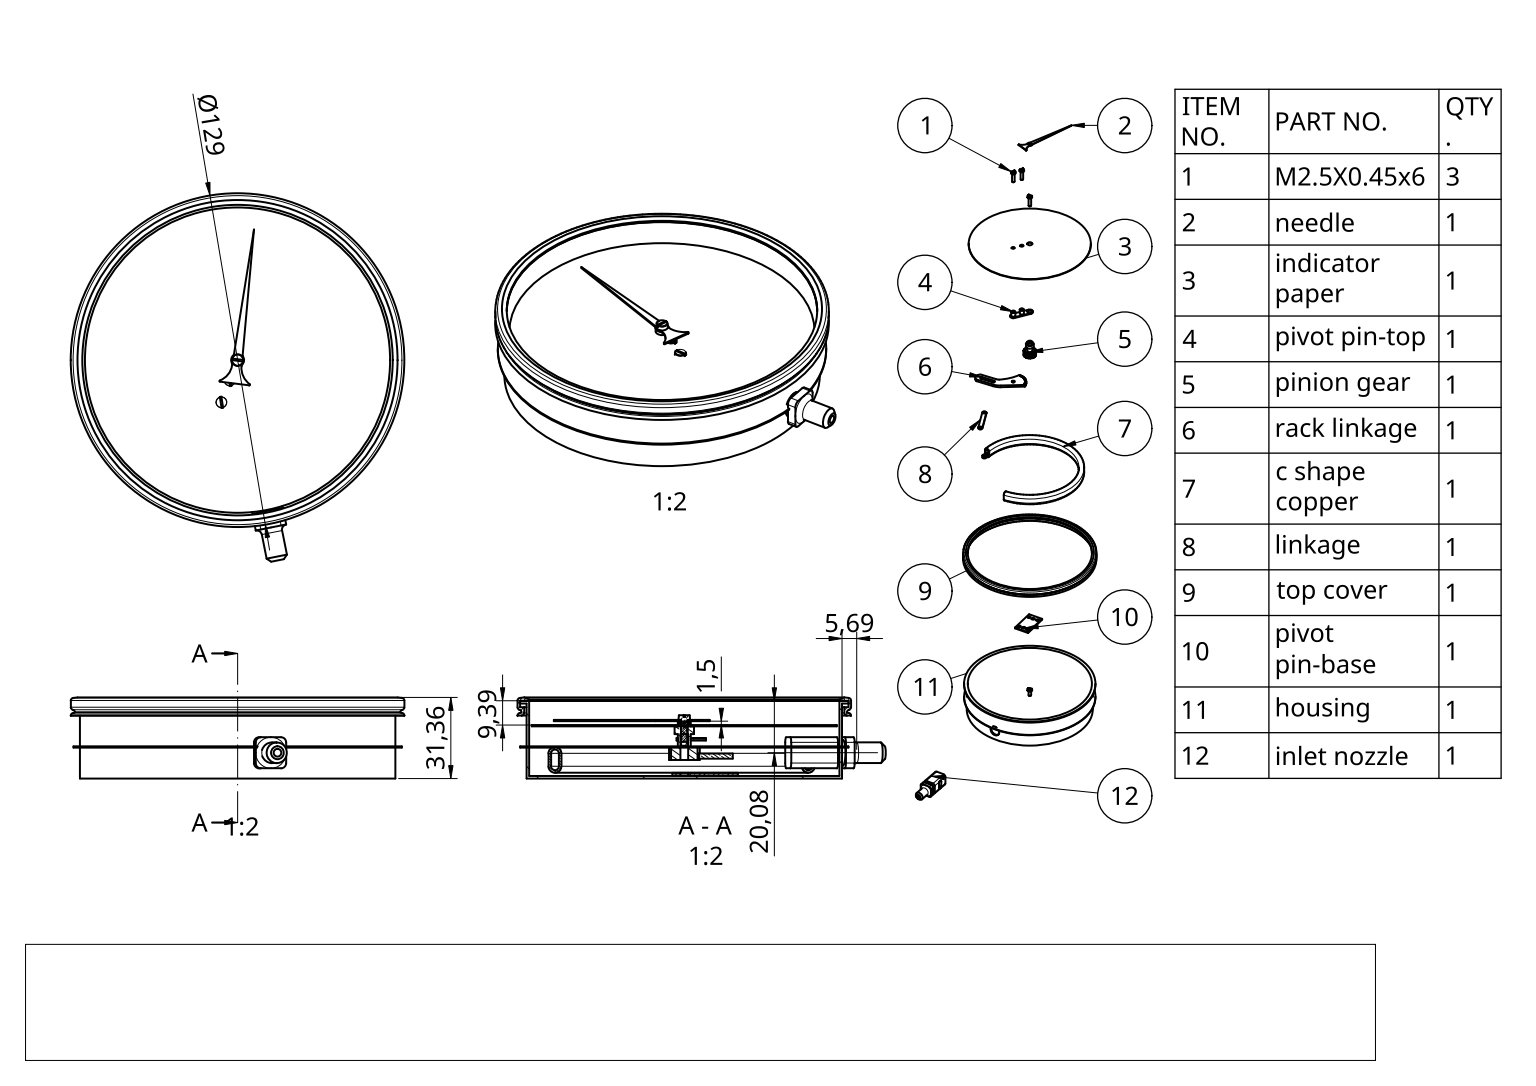
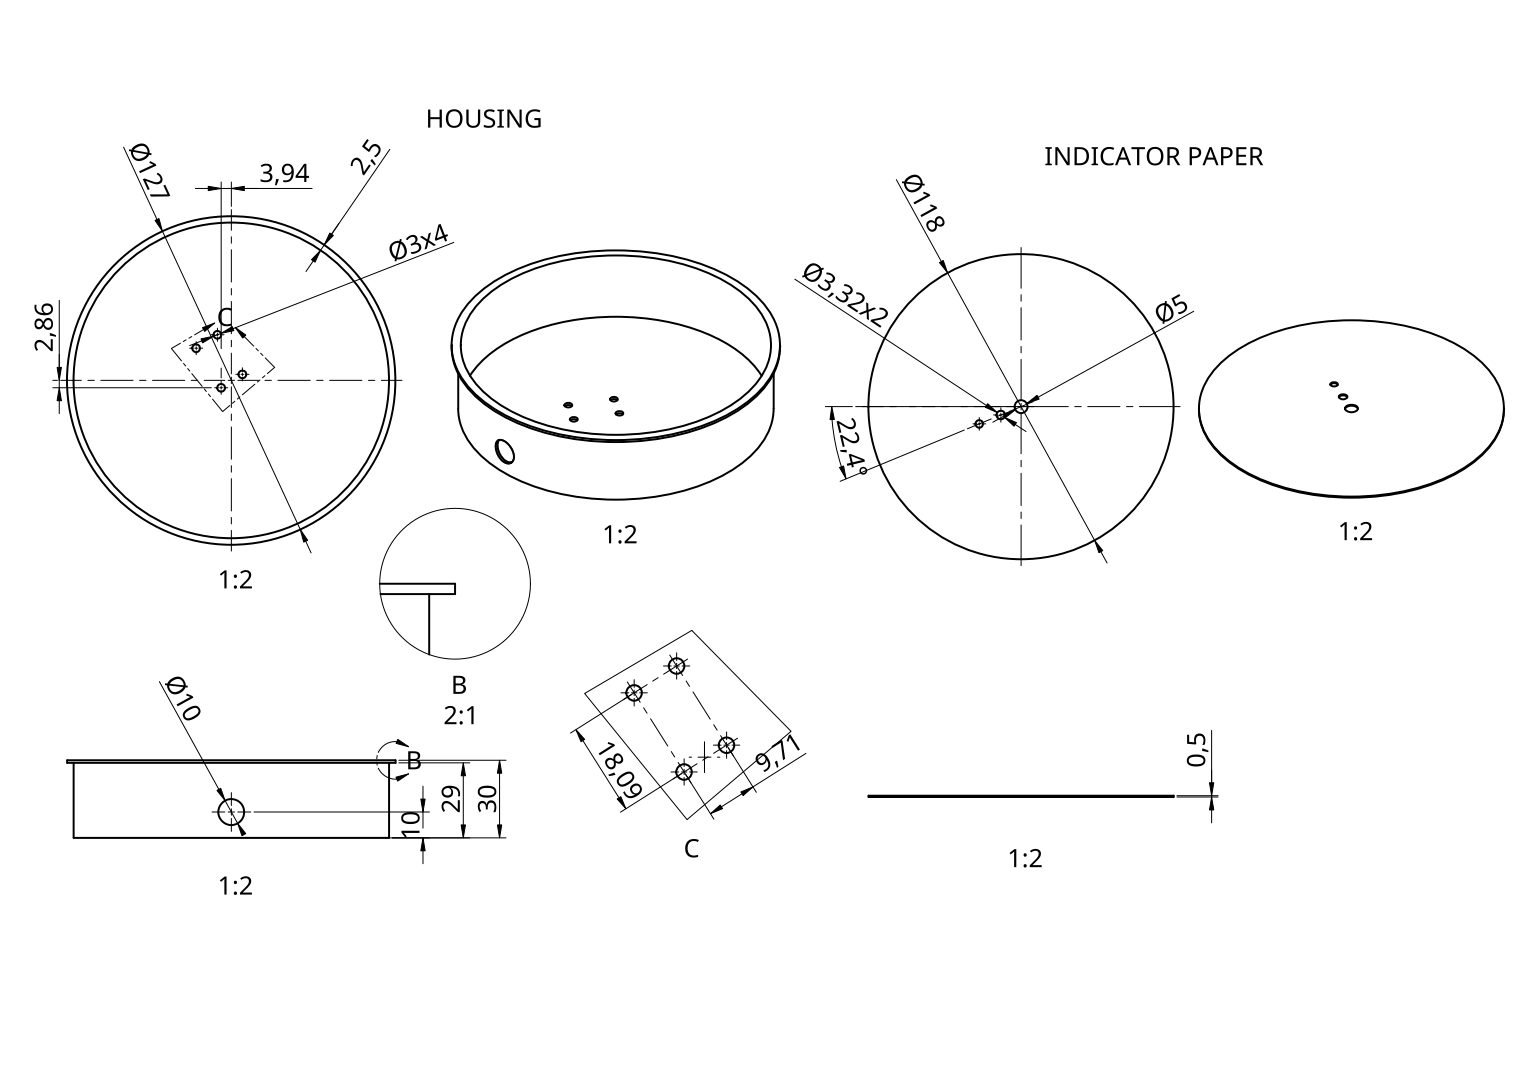
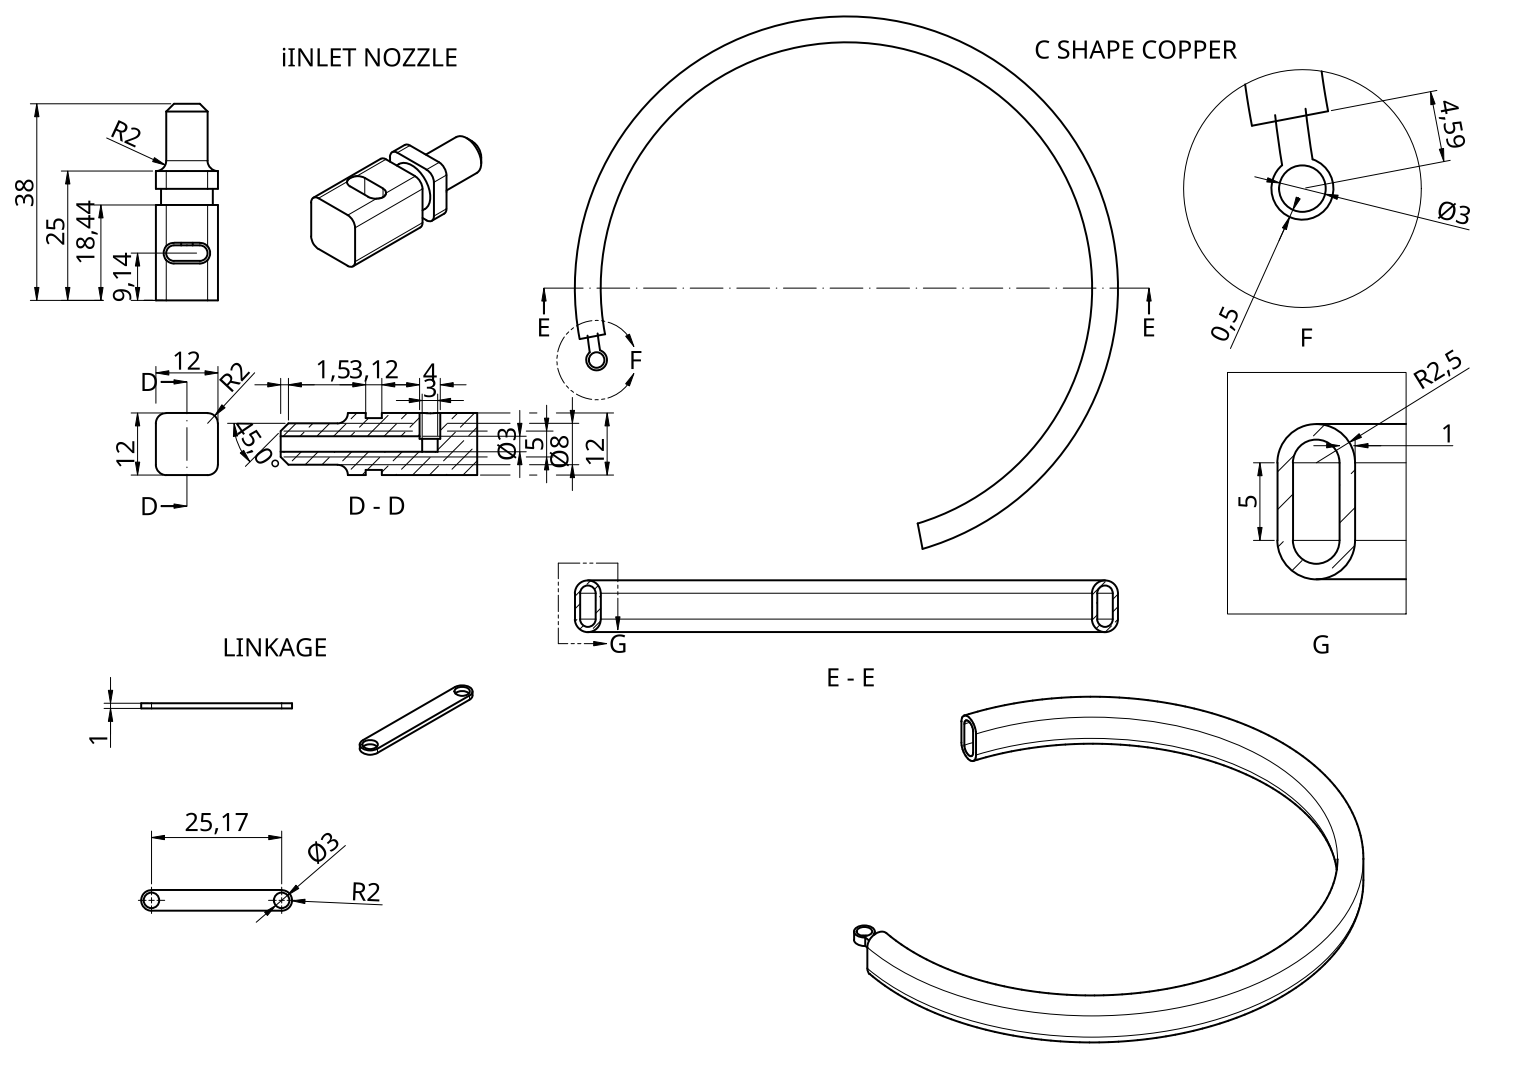
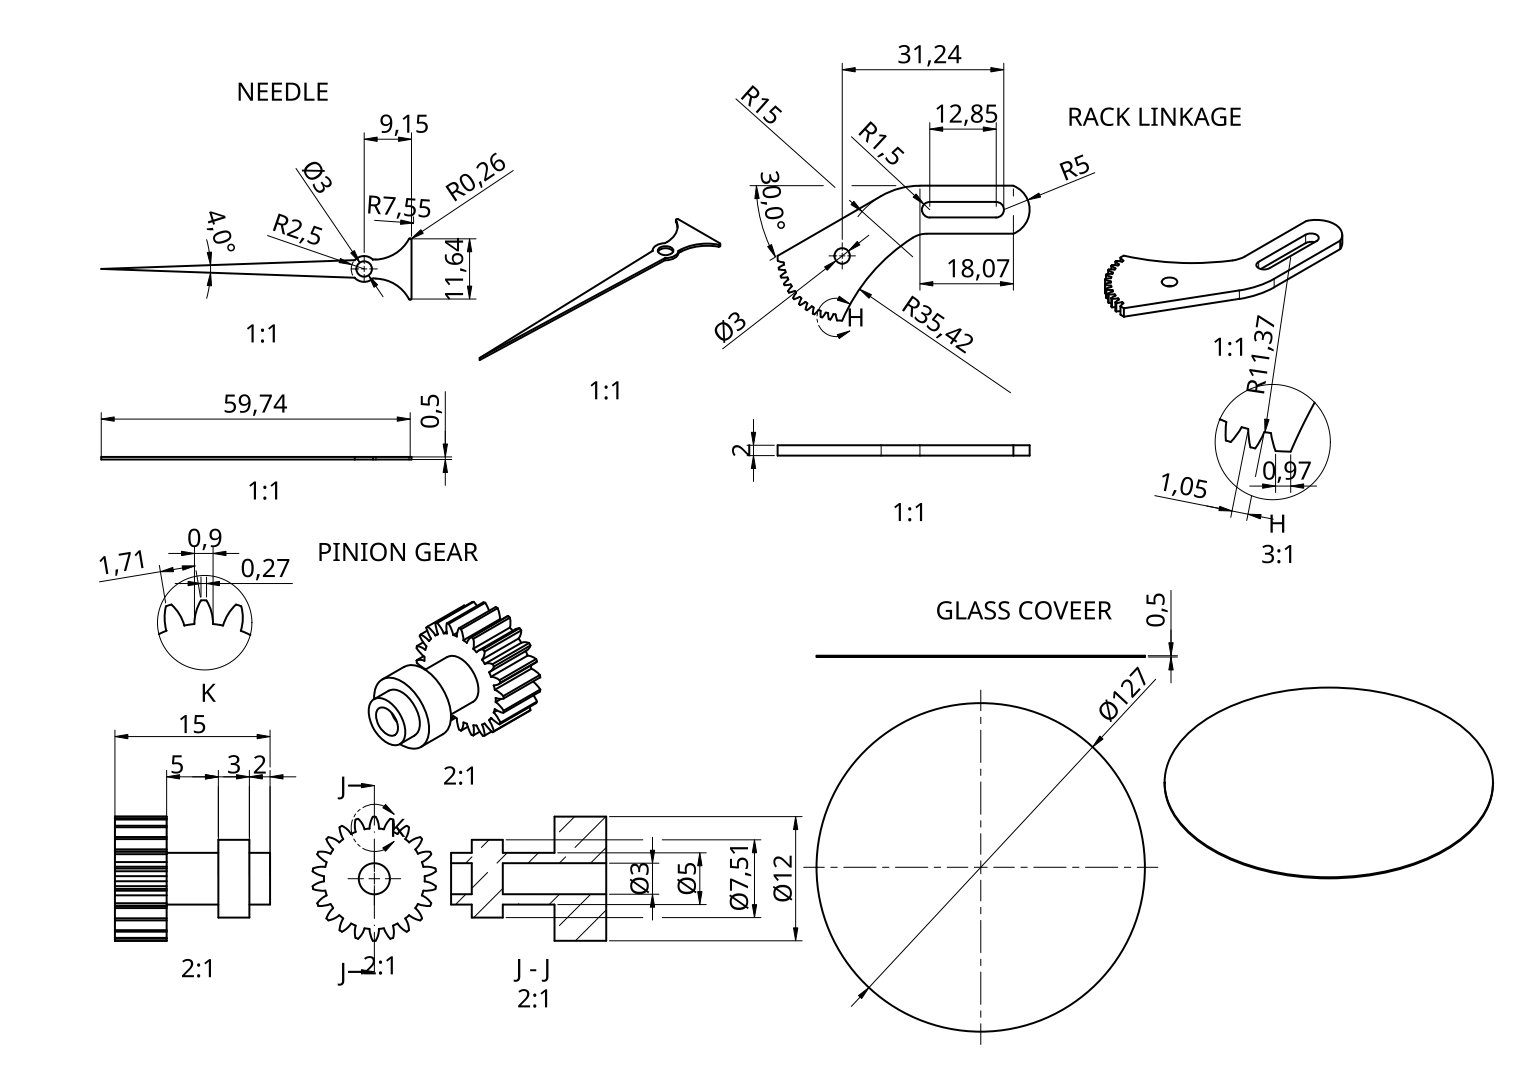
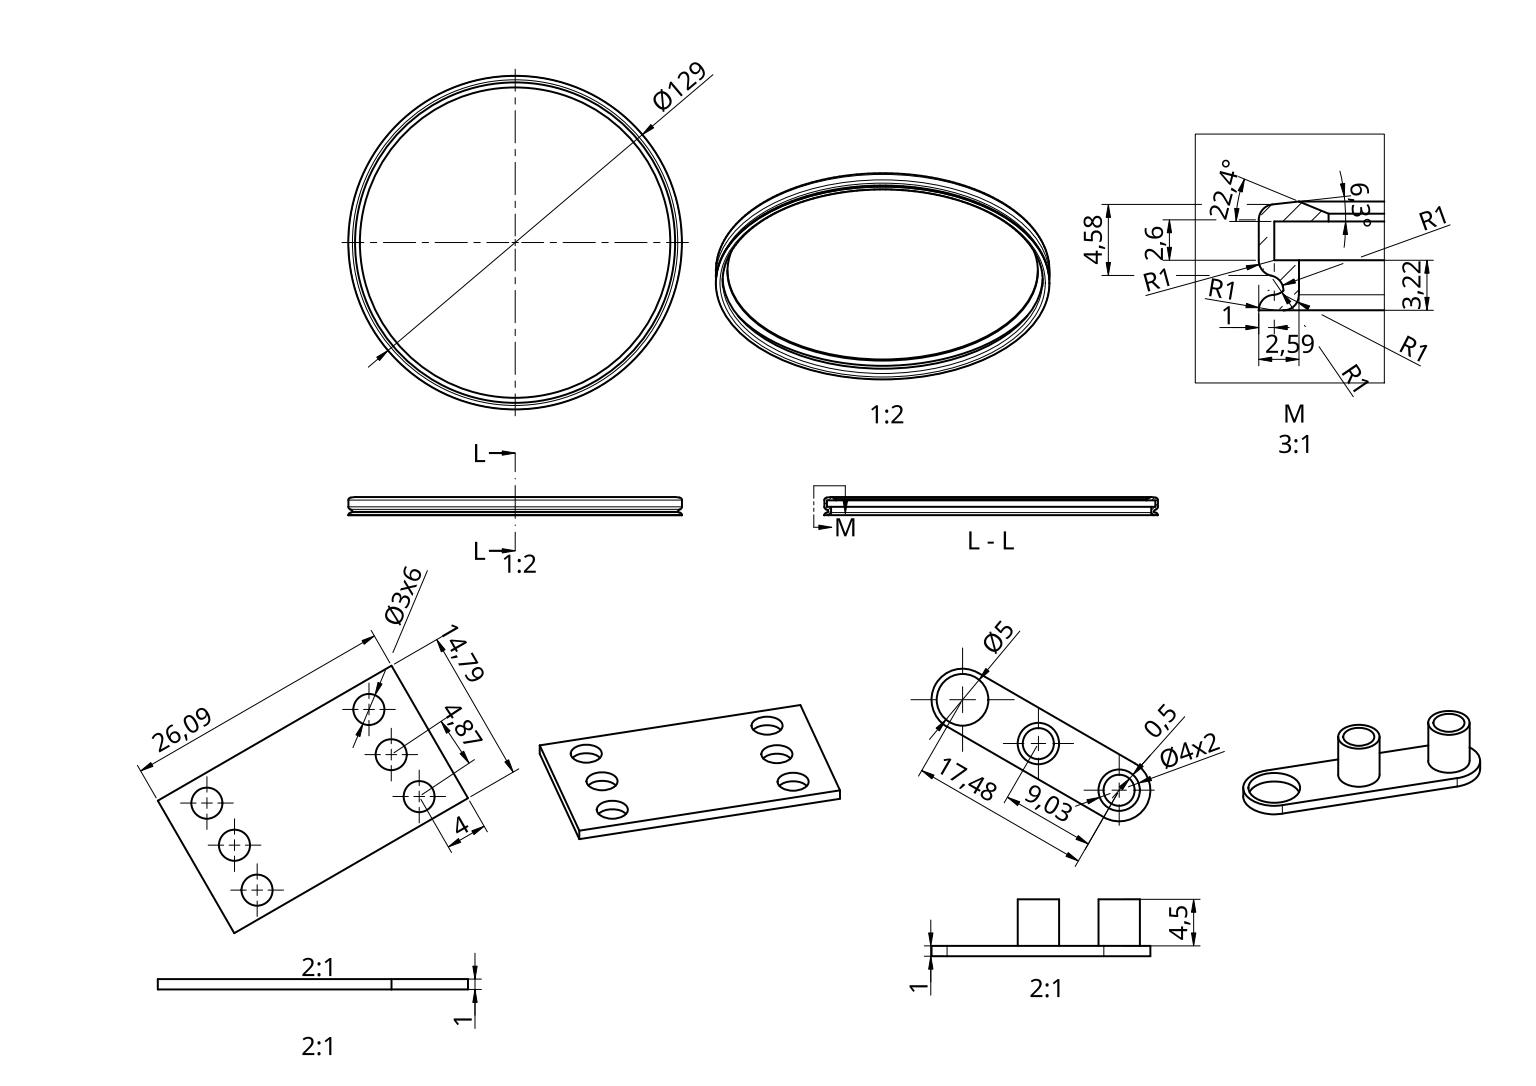
ISO-10303-21;
HEADER;
/* Generated by software containing ST-Developer
 * from STEP Tools, Inc. (www.steptools.com) 
 */
/* OPTION: using custom renumber hook */

FILE_DESCRIPTION(
/* description */ ('STEP AP242 Edition 2', 'CAx-IF Rec.Pracs.---Representation and Presentation of Product Manufa
cturing Information (PMI)---4.0---2014-10-13', 'CAx-IF Rec.Pracs.---3D Tessellated Geometry---0.4---2014-09-14', '2;1', 'CAx-IF Rec.Pracs.---User Defined Attributes---1.5---2016-08-15'),
/* implementation_level */ '2;1');

FILE_NAME(
/* name */ 'MAS-674',
/* time_stamp */ '2026-10-09T13:59:33Z',
/* author */ (''),
/* organization */ (''),
/* preprocessor_version */ 'ST-DEVELOPER v20',
/* originating_system */ 'ONSHAPE BY PTC INC, 1.221',
/* authorisation */ '  ');

FILE_SCHEMA (('AP242_MANAGED_MODEL_BASED_3D_ENGINEERING_MIM_LF { 1 0 10303 442 3 1 4 }'));
ENDSEC;

DATA;
#10=CONICAL_SURFACE('',#5743,0.00209252040565334,0.0872664625997158);
#11=CONICAL_SURFACE('',#5755,0.00100643035625,0.785398163397448);
#12=CONICAL_SURFACE('',#5977,0.0025,0.785398163397445);
#13=CONICAL_SURFACE('',#6425,0.0619081467766146,1.18042781059053);
#14=CONICAL_SURFACE('',#6427,0.0645,1.46120958979089);
#15=CONICAL_SURFACE('',#6491,0.00209252040565334,0.0872664625997158);
#16=CONICAL_SURFACE('',#6503,0.00100643035625,0.785398163397448);
#17=TOROIDAL_SURFACE('',#5734,0.0020008872882516,0.0001);
#18=TOROIDAL_SURFACE('',#5750,0.00135,0.0001);
#19=TOROIDAL_SURFACE('',#5751,0.0020008872882516,0.0001);
#20=TOROIDAL_SURFACE('',#5997,0.006,0.002);
#21=TOROIDAL_SURFACE('',#6377,0.05,0.0015);
#22=TOROIDAL_SURFACE('',#6383,0.05,0.0015);
#23=TOROIDAL_SURFACE('',#6391,0.05,0.0025);
#24=TOROIDAL_SURFACE('',#6396,0.05,0.0025);
#25=TOROIDAL_SURFACE('',#6439,0.0635,0.001);
#26=TOROIDAL_SURFACE('',#6441,0.0635,0.001);
#27=TOROIDAL_SURFACE('',#6442,0.0639081467766146,0.001);
#28=TOROIDAL_SURFACE('',#6444,0.0635863977385909,0.001);
#29=TOROIDAL_SURFACE('',#6446,0.0635,0.001);
#30=TOROIDAL_SURFACE('',#6448,0.0629081467766146,0.001);
#31=TOROIDAL_SURFACE('',#6449,0.0644389218390369,0.001);
#32=TOROIDAL_SURFACE('',#6482,0.0020008872882516,0.0001);
#33=TOROIDAL_SURFACE('',#6498,0.00135,0.0001);
#34=TOROIDAL_SURFACE('',#6499,0.0020008872882516,0.0001);
#35=LINE('',#8458,#319);
#36=LINE('',#8486,#320);
#37=LINE('',#8529,#321);
#38=LINE('',#8530,#322);
#39=LINE('',#8540,#323);
#40=LINE('',#8544,#324);
#41=LINE('',#8549,#325);
#42=LINE('',#8553,#326);
#43=LINE('',#8560,#327);
#44=LINE('',#8565,#328);
#45=LINE('',#8653,#329);
#46=LINE('',#8657,#330);
#47=LINE('',#8661,#331);
#48=LINE('',#8673,#332);
#49=LINE('',#8677,#333);
#50=LINE('',#8681,#334);
#51=LINE('',#8768,#335);
#52=LINE('',#8772,#336);
#53=LINE('',#8774,#337);
#54=LINE('',#8776,#338);
#55=LINE('',#8778,#339);
#56=LINE('',#8780,#340);
#57=LINE('',#8782,#341);
#58=LINE('',#8784,#342);
#59=LINE('',#8787,#343);
#60=LINE('',#8788,#344);
#61=LINE('',#8790,#345);
#62=LINE('',#8792,#346);
#63=LINE('',#8795,#347);
#64=LINE('',#8796,#348);
#65=LINE('',#8798,#349);
#66=LINE('',#8799,#350);
#67=LINE('',#8801,#351);
#68=LINE('',#8802,#352);
#69=LINE('',#8804,#353);
#70=LINE('',#8805,#354);
#71=LINE('',#8807,#355);
#72=LINE('',#8808,#356);
#73=LINE('',#8810,#357);
#74=LINE('',#8811,#358);
#75=LINE('',#8813,#359);
#76=LINE('',#8814,#360);
#77=LINE('',#8816,#361);
#78=LINE('',#8817,#362);
#79=LINE('',#8819,#363);
#80=LINE('',#8820,#364);
#81=LINE('',#8822,#365);
#82=LINE('',#8823,#366);
#83=LINE('',#8825,#367);
#84=LINE('',#8827,#368);
#85=LINE('',#8830,#369);
#86=LINE('',#8832,#370);
#87=LINE('',#8835,#371);
#88=LINE('',#8837,#372);
#89=LINE('',#8840,#373);
#90=LINE('',#8842,#374);
#91=LINE('',#8845,#375);
#92=LINE('',#8847,#376);
#93=LINE('',#8850,#377);
#94=LINE('',#8852,#378);
#95=LINE('',#8855,#379);
#96=LINE('',#8857,#380);
#97=LINE('',#8860,#381);
#98=LINE('',#8862,#382);
#99=LINE('',#8865,#383);
#100=LINE('',#8867,#384);
#101=LINE('',#8870,#385);
#102=LINE('',#8872,#386);
#103=LINE('',#8875,#387);
#104=LINE('',#8877,#388);
#105=LINE('',#8882,#389);
#106=LINE('',#8885,#390);
#107=LINE('',#8887,#391);
#108=LINE('',#8889,#392);
#109=LINE('',#8891,#393);
#110=LINE('',#8894,#394);
#111=LINE('',#8896,#395);
#112=LINE('',#8898,#396);
#113=LINE('',#8900,#397);
#114=LINE('',#8902,#398);
#115=LINE('',#8905,#399);
#116=LINE('',#8909,#400);
#117=LINE('',#8913,#401);
#118=LINE('',#8915,#402);
#119=LINE('',#8918,#403);
#120=LINE('',#8920,#404);
#121=LINE('',#8922,#405);
#122=LINE('',#8924,#406);
#123=LINE('',#8926,#407);
#124=LINE('',#8929,#408);
#125=LINE('',#8931,#409);
#126=LINE('',#8933,#410);
#127=LINE('',#8935,#411);
#128=LINE('',#8938,#412);
#129=LINE('',#8940,#413);
#130=LINE('',#8942,#414);
#131=LINE('',#8944,#415);
#132=LINE('',#8946,#416);
#133=LINE('',#8949,#417);
#134=LINE('',#8951,#418);
#135=LINE('',#8953,#419);
#136=LINE('',#8955,#420);
#137=LINE('',#8958,#421);
#138=LINE('',#8960,#422);
#139=LINE('',#8962,#423);
#140=LINE('',#8964,#424);
#141=LINE('',#8969,#425);
#142=LINE('',#8999,#426);
#143=LINE('',#9006,#427);
#144=LINE('',#9009,#428);
#145=LINE('',#9019,#429);
#146=LINE('',#9024,#430);
#147=LINE('',#9026,#431);
#148=LINE('',#9042,#432);
#149=LINE('',#9046,#433);
#150=LINE('',#9048,#434);
#151=LINE('',#9052,#435);
#152=LINE('',#9054,#436);
#153=LINE('',#9058,#437);
#154=LINE('',#9060,#438);
#155=LINE('',#9062,#439);
#156=LINE('',#9065,#440);
#157=LINE('',#9069,#441);
#158=LINE('',#9071,#442);
#159=LINE('',#9073,#443);
#160=LINE('',#9077,#444);
#161=LINE('',#9079,#445);
#162=LINE('',#9084,#446);
#163=LINE('',#9086,#447);
#164=LINE('',#9106,#448);
#165=LINE('',#9110,#449);
#166=LINE('',#9117,#450);
#167=LINE('',#9121,#451);
#168=LINE('',#9125,#452);
#169=LINE('',#9126,#453);
#170=LINE('',#9128,#454);
#171=LINE('',#9130,#455);
#172=LINE('',#9155,#456);
#173=LINE('',#9158,#457);
#174=LINE('',#9160,#458);
#175=LINE('',#9162,#459);
#176=LINE('',#9164,#460);
#177=LINE('',#9166,#461);
#178=LINE('',#9168,#462);
#179=LINE('',#9170,#463);
#180=LINE('',#9172,#464);
#181=LINE('',#9174,#465);
#182=LINE('',#9181,#466);
#183=LINE('',#9182,#467);
#184=LINE('',#9422,#468);
#185=LINE('',#9424,#469);
#186=LINE('',#9428,#470);
#187=LINE('',#9432,#471);
#188=LINE('',#9434,#472);
#189=LINE('',#9436,#473);
#190=LINE('',#9440,#474);
#191=LINE('',#9442,#475);
#192=LINE('',#9446,#476);
#193=LINE('',#9448,#477);
#194=LINE('',#9452,#478);
#195=LINE('',#9456,#479);
#196=LINE('',#9458,#480);
#197=LINE('',#9460,#481);
#198=LINE('',#9464,#482);
#199=LINE('',#9468,#483);
#200=LINE('',#9470,#484);
#201=LINE('',#9472,#485);
#202=LINE('',#9476,#486);
#203=LINE('',#9478,#487);
#204=LINE('',#9482,#488);
#205=LINE('',#9486,#489);
#206=LINE('',#9488,#490);
#207=LINE('',#9490,#491);
#208=LINE('',#9494,#492);
#209=LINE('',#9498,#493);
#210=LINE('',#9500,#494);
#211=LINE('',#9504,#495);
#212=LINE('',#9506,#496);
#213=LINE('',#9510,#497);
#214=LINE('',#9512,#498);
#215=LINE('',#9514,#499);
#216=LINE('',#9518,#500);
#217=LINE('',#9520,#501);
#218=LINE('',#9524,#502);
#219=LINE('',#9528,#503);
#220=LINE('',#9530,#504);
#221=LINE('',#9534,#505);
#222=LINE('',#9536,#506);
#223=LINE('',#9540,#507);
#224=LINE('',#9542,#508);
#225=LINE('',#9544,#509);
#226=LINE('',#9662,#510);
#227=LINE('',#9663,#511);
#228=LINE('',#9665,#512);
#229=LINE('',#9667,#513);
#230=LINE('',#9670,#514);
#231=LINE('',#9672,#515);
#232=LINE('',#9675,#516);
#233=LINE('',#9677,#517);
#234=LINE('',#9680,#518);
#235=LINE('',#9682,#519);
#236=LINE('',#9685,#520);
#237=LINE('',#9687,#521);
#238=LINE('',#9690,#522);
#239=LINE('',#9692,#523);
#240=LINE('',#9695,#524);
#241=LINE('',#9697,#525);
#242=LINE('',#9700,#526);
#243=LINE('',#9702,#527);
#244=LINE('',#9705,#528);
#245=LINE('',#9707,#529);
#246=LINE('',#9710,#530);
#247=LINE('',#9712,#531);
#248=LINE('',#9715,#532);
#249=LINE('',#9717,#533);
#250=LINE('',#9720,#534);
#251=LINE('',#9722,#535);
#252=LINE('',#9725,#536);
#253=LINE('',#9727,#537);
#254=LINE('',#9730,#538);
#255=LINE('',#9732,#539);
#256=LINE('',#9735,#540);
#257=LINE('',#9737,#541);
#258=LINE('',#9740,#542);
#259=LINE('',#9742,#543);
#260=LINE('',#9745,#544);
#261=LINE('',#9747,#545);
#262=LINE('',#9750,#546);
#263=LINE('',#9752,#547);
#264=LINE('',#9755,#548);
#265=LINE('',#9757,#549);
#266=LINE('',#9760,#550);
#267=LINE('',#9762,#551);
#268=LINE('',#9765,#552);
#269=LINE('',#9767,#553);
#270=LINE('',#9770,#554);
#271=LINE('',#9772,#555);
#272=LINE('',#9799,#556);
#273=LINE('',#9803,#557);
#274=LINE('',#9807,#558);
#275=LINE('',#9813,#559);
#276=LINE('',#9817,#560);
#277=LINE('',#9818,#561);
#278=LINE('',#9843,#562);
#279=LINE('',#9847,#563);
#280=LINE('',#9861,#564);
#281=LINE('',#9862,#565);
#282=LINE('',#9873,#566);
#283=LINE('',#9883,#567);
#284=LINE('',#9888,#568);
#285=LINE('',#9892,#569);
#286=LINE('',#9909,#570);
#287=LINE('',#9913,#571);
#288=LINE('',#9920,#572);
#289=LINE('',#9924,#573);
#290=LINE('',#9930,#574);
#291=LINE('',#9931,#575);
#292=LINE('',#9933,#576);
#293=LINE('',#9935,#577);
#294=LINE('',#9995,#578);
#295=LINE('',#9999,#579);
#296=LINE('',#10001,#580);
#297=LINE('',#10005,#581);
#298=LINE('',#10011,#582);
#299=LINE('',#10018,#583);
#300=LINE('',#10024,#584);
#301=LINE('',#10028,#585);
#302=LINE('',#10030,#586);
#303=LINE('',#10034,#587);
#304=LINE('',#10040,#588);
#305=LINE('',#10041,#589);
#306=LINE('',#10043,#590);
#307=LINE('',#10045,#591);
#308=LINE('',#10047,#592);
#309=LINE('',#10049,#593);
#310=LINE('',#10051,#594);
#311=LINE('',#10053,#595);
#312=LINE('',#10055,#596);
#313=LINE('',#10057,#597);
#314=LINE('',#10059,#598);
#315=LINE('',#10064,#599);
#316=LINE('',#10092,#600);
#317=LINE('',#10135,#601);
#318=LINE('',#10136,#602);
#319=VECTOR('',#6563,1.);
#320=VECTOR('',#6584,1.);
#321=VECTOR('',#6605,1.);
#322=VECTOR('',#6606,1.);
#323=VECTOR('',#6621,1.);
#324=VECTOR('',#6624,1.);
#325=VECTOR('',#6629,1.);
#326=VECTOR('',#6632,1.);
#327=VECTOR('',#6641,1.);
#328=VECTOR('',#6644,1.);
#329=VECTOR('',#6733,1.);
#330=VECTOR('',#6736,1.);
#331=VECTOR('',#6739,1.);
#332=VECTOR('',#6752,1.);
#333=VECTOR('',#6755,1.);
#334=VECTOR('',#6758,1.);
#335=VECTOR('',#6845,1.);
#336=VECTOR('',#6848,1.);
#337=VECTOR('',#6851,1.);
#338=VECTOR('',#6854,1.);
#339=VECTOR('',#6857,1.);
#340=VECTOR('',#6860,1.);
#341=VECTOR('',#6863,1.);
#342=VECTOR('',#6866,1.);
#343=VECTOR('',#6871,1.);
#344=VECTOR('',#6872,1.);
#345=VECTOR('',#6875,1.);
#346=VECTOR('',#6878,1.);
#347=VECTOR('',#6883,1.);
#348=VECTOR('',#6884,1.);
#349=VECTOR('',#6887,1.);
#350=VECTOR('',#6888,1.);
#351=VECTOR('',#6891,1.);
#352=VECTOR('',#6892,1.);
#353=VECTOR('',#6895,1.);
#354=VECTOR('',#6896,1.);
#355=VECTOR('',#6899,1.);
#356=VECTOR('',#6900,1.);
#357=VECTOR('',#6903,1.);
#358=VECTOR('',#6904,1.);
#359=VECTOR('',#6907,1.);
#360=VECTOR('',#6908,1.);
#361=VECTOR('',#6911,1.);
#362=VECTOR('',#6912,1.);
#363=VECTOR('',#6915,1.);
#364=VECTOR('',#6916,1.);
#365=VECTOR('',#6919,1.);
#366=VECTOR('',#6920,1.);
#367=VECTOR('',#6923,1.);
#368=VECTOR('',#6926,1.);
#369=VECTOR('',#6931,1.);
#370=VECTOR('',#6934,1.);
#371=VECTOR('',#6939,1.);
#372=VECTOR('',#6942,1.);
#373=VECTOR('',#6947,1.);
#374=VECTOR('',#6950,1.);
#375=VECTOR('',#6955,1.);
#376=VECTOR('',#6958,1.);
#377=VECTOR('',#6963,1.);
#378=VECTOR('',#6966,1.);
#379=VECTOR('',#6971,1.);
#380=VECTOR('',#6974,1.);
#381=VECTOR('',#6979,1.);
#382=VECTOR('',#6982,1.);
#383=VECTOR('',#6987,1.);
#384=VECTOR('',#6990,1.);
#385=VECTOR('',#6995,1.);
#386=VECTOR('',#6998,1.);
#387=VECTOR('',#7003,1.);
#388=VECTOR('',#7006,1.);
#389=VECTOR('',#7015,1.);
#390=VECTOR('',#7016,1.);
#391=VECTOR('',#7017,1.);
#392=VECTOR('',#7018,1.);
#393=VECTOR('',#7021,1.);
#394=VECTOR('',#7022,1.);
#395=VECTOR('',#7023,1.);
#396=VECTOR('',#7024,1.);
#397=VECTOR('',#7025,1.);
#398=VECTOR('',#7028,1.);
#399=VECTOR('',#7029,1.);
#400=VECTOR('',#7032,1.);
#401=VECTOR('',#7035,1.);
#402=VECTOR('',#7038,1.);
#403=VECTOR('',#7039,1.);
#404=VECTOR('',#7040,1.);
#405=VECTOR('',#7041,1.);
#406=VECTOR('',#7042,1.);
#407=VECTOR('',#7045,1.);
#408=VECTOR('',#7046,1.);
#409=VECTOR('',#7047,1.);
#410=VECTOR('',#7048,1.);
#411=VECTOR('',#7051,1.);
#412=VECTOR('',#7052,1.);
#413=VECTOR('',#7053,1.);
#414=VECTOR('',#7054,1.);
#415=VECTOR('',#7055,1.);
#416=VECTOR('',#7058,1.);
#417=VECTOR('',#7059,1.);
#418=VECTOR('',#7060,1.);
#419=VECTOR('',#7061,1.);
#420=VECTOR('',#7064,1.);
#421=VECTOR('',#7065,1.);
#422=VECTOR('',#7066,1.);
#423=VECTOR('',#7067,1.);
#424=VECTOR('',#7068,1.);
#425=VECTOR('',#7075,1.);
#426=VECTOR('',#7110,1.);
#427=VECTOR('',#7121,1.);
#428=VECTOR('',#7124,1.);
#429=VECTOR('',#7141,1.);
#430=VECTOR('',#7144,1.);
#431=VECTOR('',#7145,1.);
#432=VECTOR('',#7168,1.);
#433=VECTOR('',#7171,1.);
#434=VECTOR('',#7174,1.);
#435=VECTOR('',#7177,1.);
#436=VECTOR('',#7178,1.);
#437=VECTOR('',#7183,1.);
#438=VECTOR('',#7186,1.);
#439=VECTOR('',#7189,1.);
#440=VECTOR('',#7192,1.);
#441=VECTOR('',#7195,1.);
#442=VECTOR('',#7196,1.);
#443=VECTOR('',#7199,1.);
#444=VECTOR('',#7202,1.);
#445=VECTOR('',#7205,1.);
#446=VECTOR('',#7212,1.);
#447=VECTOR('',#7215,1.);
#448=VECTOR('',#7242,1.);
#449=VECTOR('',#7245,1.);
#450=VECTOR('',#7252,1.);
#451=VECTOR('',#7255,1.);
#452=VECTOR('',#7260,1.);
#453=VECTOR('',#7261,1.);
#454=VECTOR('',#7264,1.);
#455=VECTOR('',#7267,1.);
#456=VECTOR('',#7304,1.);
#457=VECTOR('',#7305,1.);
#458=VECTOR('',#7306,1.);
#459=VECTOR('',#7307,1.);
#460=VECTOR('',#7310,1.);
#461=VECTOR('',#7311,1.);
#462=VECTOR('',#7312,1.);
#463=VECTOR('',#7315,1.);
#464=VECTOR('',#7316,1.);
#465=VECTOR('',#7317,1.);
#466=VECTOR('',#7326,1.);
#467=VECTOR('',#7327,1.);
#468=VECTOR('',#7586,1.);
#469=VECTOR('',#7587,1.);
#470=VECTOR('',#7592,1.);
#471=VECTOR('',#7595,1.);
#472=VECTOR('',#7598,1.);
#473=VECTOR('',#7599,1.);
#474=VECTOR('',#7604,1.);
#475=VECTOR('',#7605,1.);
#476=VECTOR('',#7610,1.);
#477=VECTOR('',#7611,1.);
#478=VECTOR('',#7616,1.);
#479=VECTOR('',#7619,1.);
#480=VECTOR('',#7622,1.);
#481=VECTOR('',#7623,1.);
#482=VECTOR('',#7628,1.);
#483=VECTOR('',#7631,1.);
#484=VECTOR('',#7634,1.);
#485=VECTOR('',#7635,1.);
#486=VECTOR('',#7640,1.);
#487=VECTOR('',#7641,1.);
#488=VECTOR('',#7646,1.);
#489=VECTOR('',#7649,1.);
#490=VECTOR('',#7652,1.);
#491=VECTOR('',#7653,1.);
#492=VECTOR('',#7658,1.);
#493=VECTOR('',#7661,1.);
#494=VECTOR('',#7664,1.);
#495=VECTOR('',#7667,1.);
#496=VECTOR('',#7670,1.);
#497=VECTOR('',#7673,1.);
#498=VECTOR('',#7676,1.);
#499=VECTOR('',#7677,1.);
#500=VECTOR('',#7682,1.);
#501=VECTOR('',#7683,1.);
#502=VECTOR('',#7688,1.);
#503=VECTOR('',#7691,1.);
#504=VECTOR('',#7694,1.);
#505=VECTOR('',#7697,1.);
#506=VECTOR('',#7700,1.);
#507=VECTOR('',#7703,1.);
#508=VECTOR('',#7706,1.);
#509=VECTOR('',#7707,1.);
#510=VECTOR('',#7848,1.);
#511=VECTOR('',#7849,1.);
#512=VECTOR('',#7852,1.);
#513=VECTOR('',#7855,1.);
#514=VECTOR('',#7860,1.);
#515=VECTOR('',#7863,1.);
#516=VECTOR('',#7868,1.);
#517=VECTOR('',#7871,1.);
#518=VECTOR('',#7876,1.);
#519=VECTOR('',#7879,1.);
#520=VECTOR('',#7884,1.);
#521=VECTOR('',#7887,1.);
#522=VECTOR('',#7892,1.);
#523=VECTOR('',#7895,1.);
#524=VECTOR('',#7900,1.);
#525=VECTOR('',#7903,1.);
#526=VECTOR('',#7908,1.);
#527=VECTOR('',#7911,1.);
#528=VECTOR('',#7916,1.);
#529=VECTOR('',#7919,1.);
#530=VECTOR('',#7924,1.);
#531=VECTOR('',#7927,1.);
#532=VECTOR('',#7932,1.);
#533=VECTOR('',#7935,1.);
#534=VECTOR('',#7940,1.);
#535=VECTOR('',#7943,1.);
#536=VECTOR('',#7948,1.);
#537=VECTOR('',#7951,1.);
#538=VECTOR('',#7956,1.);
#539=VECTOR('',#7959,1.);
#540=VECTOR('',#7964,1.);
#541=VECTOR('',#7967,1.);
#542=VECTOR('',#7972,1.);
#543=VECTOR('',#7975,1.);
#544=VECTOR('',#7980,1.);
#545=VECTOR('',#7983,1.);
#546=VECTOR('',#7988,1.);
#547=VECTOR('',#7991,1.);
#548=VECTOR('',#7996,1.);
#549=VECTOR('',#7999,1.);
#550=VECTOR('',#8004,1.);
#551=VECTOR('',#8007,1.);
#552=VECTOR('',#8012,1.);
#553=VECTOR('',#8015,1.);
#554=VECTOR('',#8020,1.);
#555=VECTOR('',#8023,1.);
#556=VECTOR('',#8060,1.);
#557=VECTOR('',#8063,1.);
#558=VECTOR('',#8068,1.);
#559=VECTOR('',#8075,1.);
#560=VECTOR('',#8080,1.);
#561=VECTOR('',#8081,1.);
#562=VECTOR('',#8104,1.);
#563=VECTOR('',#8107,1.);
#564=VECTOR('',#8116,1.);
#565=VECTOR('',#8117,1.);
#566=VECTOR('',#8120,1.);
#567=VECTOR('',#8121,1.);
#568=VECTOR('',#8126,1.);
#569=VECTOR('',#8129,1.);
#570=VECTOR('',#8156,1.);
#571=VECTOR('',#8159,1.);
#572=VECTOR('',#8166,1.);
#573=VECTOR('',#8169,1.);
#574=VECTOR('',#8176,1.);
#575=VECTOR('',#8177,1.);
#576=VECTOR('',#8180,1.);
#577=VECTOR('',#8183,1.);
#578=VECTOR('',#8264,1.);
#579=VECTOR('',#8267,1.);
#580=VECTOR('',#8268,1.);
#581=VECTOR('',#8271,1.);
#582=VECTOR('',#8276,1.);
#583=VECTOR('',#8283,1.);
#584=VECTOR('',#8288,1.);
#585=VECTOR('',#8291,1.);
#586=VECTOR('',#8292,1.);
#587=VECTOR('',#8295,1.);
#588=VECTOR('',#8302,1.);
#589=VECTOR('',#8303,1.);
#590=VECTOR('',#8306,1.);
#591=VECTOR('',#8309,1.);
#592=VECTOR('',#8312,1.);
#593=VECTOR('',#8315,1.);
#594=VECTOR('',#8318,1.);
#595=VECTOR('',#8321,1.);
#596=VECTOR('',#8324,1.);
#597=VECTOR('',#8327,1.);
#598=VECTOR('',#8330,1.);
#599=VECTOR('',#8339,1.);
#600=VECTOR('',#8360,1.);
#601=VECTOR('',#8381,1.);
#602=VECTOR('',#8382,1.);
#603=CONTEXT_DEPENDENT_SHAPE_REPRESENTATION(#637,#10179);
#604=CONTEXT_DEPENDENT_SHAPE_REPRESENTATION(#638,#10181);
#605=CONTEXT_DEPENDENT_SHAPE_REPRESENTATION(#639,#10182);
#606=CONTEXT_DEPENDENT_SHAPE_REPRESENTATION(#640,#10184);
#607=CONTEXT_DEPENDENT_SHAPE_REPRESENTATION(#641,#10185);
#608=CONTEXT_DEPENDENT_SHAPE_REPRESENTATION(#642,#10187);
#609=CONTEXT_DEPENDENT_SHAPE_REPRESENTATION(#643,#10189);
#610=CONTEXT_DEPENDENT_SHAPE_REPRESENTATION(#644,#10191);
#611=CONTEXT_DEPENDENT_SHAPE_REPRESENTATION(#645,#10193);
#612=CONTEXT_DEPENDENT_SHAPE_REPRESENTATION(#646,#10195);
#613=CONTEXT_DEPENDENT_SHAPE_REPRESENTATION(#647,#10198);
#614=CONTEXT_DEPENDENT_SHAPE_REPRESENTATION(#648,#10200);
#615=CONTEXT_DEPENDENT_SHAPE_REPRESENTATION(#649,#10201);
#616=CONTEXT_DEPENDENT_SHAPE_REPRESENTATION(#650,#10203);
#617=CONTEXT_DEPENDENT_SHAPE_REPRESENTATION(#651,#10205);
#618=CONTEXT_DEPENDENT_SHAPE_REPRESENTATION(#652,#10207);
#619=CONTEXT_DEPENDENT_SHAPE_REPRESENTATION(#653,#10209);
#620=NEXT_ASSEMBLY_USAGE_OCCURRENCE('NAUO1','Part 1','Part 1',#10210,#10211,
'');
#621=NEXT_ASSEMBLY_USAGE_OCCURRENCE('NAUO2',
'Slotted cheese head screw M2.5x0.45 x 10',
'Slotted cheese head screw M2.5x0.45 x 10',#10210,#10212,'');
#622=NEXT_ASSEMBLY_USAGE_OCCURRENCE('NAUO3',
'Slotted cheese head screw M2.5x0.45 x 10',
'Slotted cheese head screw M2.5x0.45 x 10',#10210,#10212,'');
#623=NEXT_ASSEMBLY_USAGE_OCCURRENCE('NAUO4','Part 1','Part 1',#10210,#10213,
'');
#624=NEXT_ASSEMBLY_USAGE_OCCURRENCE('NAUO5',
'Slotted cheese head screw M2.5x0.45 x 10',
'Slotted cheese head screw M2.5x0.45 x 10',#10210,#10212,'');
#625=NEXT_ASSEMBLY_USAGE_OCCURRENCE('NAUO6','Part 1','Part 1',#10210,#10214,
'');
#626=NEXT_ASSEMBLY_USAGE_OCCURRENCE('NAUO7','Part 3','Part 3',#10210,#10215,
'');
#627=NEXT_ASSEMBLY_USAGE_OCCURRENCE('NAUO8','Part 2','Part 2',#10210,#10216,
'');
#628=NEXT_ASSEMBLY_USAGE_OCCURRENCE('NAUO9','Part 1','Part 1',#10210,#10217,
'');
#629=NEXT_ASSEMBLY_USAGE_OCCURRENCE('NAUO10','Part 1','Part 1',#10210,#10218,
'');
#630=NEXT_ASSEMBLY_USAGE_OCCURRENCE('NAUO11','Part 2','Part 2',#10219,#10220,
'');
#631=NEXT_ASSEMBLY_USAGE_OCCURRENCE('NAUO12','Part 3','Part 3',#10219,#10221,
'');
#632=NEXT_ASSEMBLY_USAGE_OCCURRENCE('NAUO13','Assembly 2 <1>',
'Assembly 2 <1>',#10210,#10219,'');
#633=NEXT_ASSEMBLY_USAGE_OCCURRENCE('NAUO14','Part 1','Part 1',#10210,#10222,
'');
#634=NEXT_ASSEMBLY_USAGE_OCCURRENCE('NAUO15','Part 1','Part 1',#10210,#10223,
'');
#635=NEXT_ASSEMBLY_USAGE_OCCURRENCE('NAUO16','Part 1','Part 1',#10210,#10224,
'');
#636=NEXT_ASSEMBLY_USAGE_OCCURRENCE('NAUO17',
'Slotted cheese head screw M2.5x0.45 x 6',
'Slotted cheese head screw M2.5x0.45 x 6',#10210,#10225,'');
#637=(
REPRESENTATION_RELATIONSHIP(' ',' ',#5689,#5688)
REPRESENTATION_RELATIONSHIP_WITH_TRANSFORMATION(#654)
SHAPE_REPRESENTATION_RELATIONSHIP()
);
#638=(
REPRESENTATION_RELATIONSHIP(' ',' ',#5690,#5688)
REPRESENTATION_RELATIONSHIP_WITH_TRANSFORMATION(#655)
SHAPE_REPRESENTATION_RELATIONSHIP()
);
#639=(
REPRESENTATION_RELATIONSHIP(' ',' ',#5690,#5688)
REPRESENTATION_RELATIONSHIP_WITH_TRANSFORMATION(#656)
SHAPE_REPRESENTATION_RELATIONSHIP()
);
#640=(
REPRESENTATION_RELATIONSHIP(' ',' ',#5691,#5688)
REPRESENTATION_RELATIONSHIP_WITH_TRANSFORMATION(#657)
SHAPE_REPRESENTATION_RELATIONSHIP()
);
#641=(
REPRESENTATION_RELATIONSHIP(' ',' ',#5690,#5688)
REPRESENTATION_RELATIONSHIP_WITH_TRANSFORMATION(#658)
SHAPE_REPRESENTATION_RELATIONSHIP()
);
#642=(
REPRESENTATION_RELATIONSHIP(' ',' ',#5692,#5688)
REPRESENTATION_RELATIONSHIP_WITH_TRANSFORMATION(#659)
SHAPE_REPRESENTATION_RELATIONSHIP()
);
#643=(
REPRESENTATION_RELATIONSHIP(' ',' ',#5693,#5688)
REPRESENTATION_RELATIONSHIP_WITH_TRANSFORMATION(#660)
SHAPE_REPRESENTATION_RELATIONSHIP()
);
#644=(
REPRESENTATION_RELATIONSHIP(' ',' ',#5694,#5688)
REPRESENTATION_RELATIONSHIP_WITH_TRANSFORMATION(#661)
SHAPE_REPRESENTATION_RELATIONSHIP()
);
#645=(
REPRESENTATION_RELATIONSHIP(' ',' ',#5695,#5688)
REPRESENTATION_RELATIONSHIP_WITH_TRANSFORMATION(#662)
SHAPE_REPRESENTATION_RELATIONSHIP()
);
#646=(
REPRESENTATION_RELATIONSHIP(' ',' ',#5696,#5688)
REPRESENTATION_RELATIONSHIP_WITH_TRANSFORMATION(#663)
SHAPE_REPRESENTATION_RELATIONSHIP()
);
#647=(
REPRESENTATION_RELATIONSHIP(' ',' ',#5698,#5697)
REPRESENTATION_RELATIONSHIP_WITH_TRANSFORMATION(#664)
SHAPE_REPRESENTATION_RELATIONSHIP()
);
#648=(
REPRESENTATION_RELATIONSHIP(' ',' ',#5699,#5697)
REPRESENTATION_RELATIONSHIP_WITH_TRANSFORMATION(#665)
SHAPE_REPRESENTATION_RELATIONSHIP()
);
#649=(
REPRESENTATION_RELATIONSHIP(' ',' ',#5697,#5688)
REPRESENTATION_RELATIONSHIP_WITH_TRANSFORMATION(#666)
SHAPE_REPRESENTATION_RELATIONSHIP()
);
#650=(
REPRESENTATION_RELATIONSHIP(' ',' ',#5700,#5688)
REPRESENTATION_RELATIONSHIP_WITH_TRANSFORMATION(#667)
SHAPE_REPRESENTATION_RELATIONSHIP()
);
#651=(
REPRESENTATION_RELATIONSHIP(' ',' ',#5701,#5688)
REPRESENTATION_RELATIONSHIP_WITH_TRANSFORMATION(#668)
SHAPE_REPRESENTATION_RELATIONSHIP()
);
#652=(
REPRESENTATION_RELATIONSHIP(' ',' ',#5702,#5688)
REPRESENTATION_RELATIONSHIP_WITH_TRANSFORMATION(#669)
SHAPE_REPRESENTATION_RELATIONSHIP()
);
#653=(
REPRESENTATION_RELATIONSHIP(' ',' ',#5703,#5688)
REPRESENTATION_RELATIONSHIP_WITH_TRANSFORMATION(#670)
SHAPE_REPRESENTATION_RELATIONSHIP()
);
#654=ITEM_DEFINED_TRANSFORMATION(' ',' ',#5704,#5731);
#655=ITEM_DEFINED_TRANSFORMATION(' ',' ',#5704,#5756);
#656=ITEM_DEFINED_TRANSFORMATION(' ',' ',#5704,#5757);
#657=ITEM_DEFINED_TRANSFORMATION(' ',' ',#5704,#5921);
#658=ITEM_DEFINED_TRANSFORMATION(' ',' ',#5704,#5922);
#659=ITEM_DEFINED_TRANSFORMATION(' ',' ',#5704,#6003);
#660=ITEM_DEFINED_TRANSFORMATION(' ',' ',#5704,#6033);
#661=ITEM_DEFINED_TRANSFORMATION(' ',' ',#5704,#6058);
#662=ITEM_DEFINED_TRANSFORMATION(' ',' ',#5704,#6073);
#663=ITEM_DEFINED_TRANSFORMATION(' ',' ',#5704,#6360);
#664=ITEM_DEFINED_TRANSFORMATION(' ',' ',#5704,#6376);
#665=ITEM_DEFINED_TRANSFORMATION(' ',' ',#5704,#6399);
#666=ITEM_DEFINED_TRANSFORMATION(' ',' ',#5704,#6400);
#667=ITEM_DEFINED_TRANSFORMATION(' ',' ',#5704,#6417);
#668=ITEM_DEFINED_TRANSFORMATION(' ',' ',#5704,#6450);
#669=ITEM_DEFINED_TRANSFORMATION(' ',' ',#5704,#6479);
#670=ITEM_DEFINED_TRANSFORMATION(' ',' ',#5704,#6504);
#671=SHAPE_REPRESENTATION_RELATIONSHIP('','',#5689,#685);
#672=SHAPE_REPRESENTATION_RELATIONSHIP('','',#5690,#686);
#673=SHAPE_REPRESENTATION_RELATIONSHIP('','',#5691,#687);
#674=SHAPE_REPRESENTATION_RELATIONSHIP('','',#5692,#688);
#675=SHAPE_REPRESENTATION_RELATIONSHIP('','',#5693,#689);
#676=SHAPE_REPRESENTATION_RELATIONSHIP('','',#5694,#690);
#677=SHAPE_REPRESENTATION_RELATIONSHIP('','',#5695,#691);
#678=SHAPE_REPRESENTATION_RELATIONSHIP('','',#5696,#692);
#679=SHAPE_REPRESENTATION_RELATIONSHIP('','',#5698,#693);
#680=SHAPE_REPRESENTATION_RELATIONSHIP('','',#5699,#694);
#681=SHAPE_REPRESENTATION_RELATIONSHIP('','',#5700,#695);
#682=SHAPE_REPRESENTATION_RELATIONSHIP('','',#5701,#696);
#683=SHAPE_REPRESENTATION_RELATIONSHIP('','',#5702,#697);
#684=SHAPE_REPRESENTATION_RELATIONSHIP('','',#5703,#698);
#685=ADVANCED_BREP_SHAPE_REPRESENTATION('',(#5658),#10143);
#686=ADVANCED_BREP_SHAPE_REPRESENTATION('',(#5659),#10144);
#687=ADVANCED_BREP_SHAPE_REPRESENTATION('',(#5660),#10145);
#688=ADVANCED_BREP_SHAPE_REPRESENTATION('',(#5661),#10146);
#689=ADVANCED_BREP_SHAPE_REPRESENTATION('',(#5662),#10147);
#690=ADVANCED_BREP_SHAPE_REPRESENTATION('',(#5663),#10148);
#691=ADVANCED_BREP_SHAPE_REPRESENTATION('',(#5664),#10149);
#692=ADVANCED_BREP_SHAPE_REPRESENTATION('',(#5665),#10150);
#693=ADVANCED_BREP_SHAPE_REPRESENTATION('',(#5666),#10152);
#694=ADVANCED_BREP_SHAPE_REPRESENTATION('',(#5667),#10153);
#695=ADVANCED_BREP_SHAPE_REPRESENTATION('',(#5668),#10154);
#696=ADVANCED_BREP_SHAPE_REPRESENTATION('',(#5669),#10155);
#697=ADVANCED_BREP_SHAPE_REPRESENTATION('',(#5670),#10156);
#698=ADVANCED_BREP_SHAPE_REPRESENTATION('',(#5671),#10157);
#699=PLANE('',#5711);
#700=PLANE('',#5713);
#701=PLANE('',#5720);
#702=PLANE('',#5721);
#703=PLANE('',#5732);
#704=PLANE('',#5740);
#705=PLANE('',#5742);
#706=PLANE('',#5748);
#707=PLANE('',#5752);
#708=PLANE('',#5753);
#709=PLANE('',#5754);
#710=PLANE('',#5767);
#711=PLANE('',#5817);
#712=PLANE('',#5867);
#713=PLANE('',#5870);
#714=PLANE('',#5872);
#715=PLANE('',#5875);
#716=PLANE('',#5877);
#717=PLANE('',#5923);
#718=PLANE('',#5924);
#719=PLANE('',#5925);
#720=PLANE('',#5928);
#721=PLANE('',#5929);
#722=PLANE('',#5930);
#723=PLANE('',#5931);
#724=PLANE('',#5932);
#725=PLANE('',#5957);
#726=PLANE('',#5960);
#727=PLANE('',#5962);
#728=PLANE('',#5964);
#729=PLANE('',#5966);
#730=PLANE('',#5968);
#731=PLANE('',#5970);
#732=PLANE('',#5974);
#733=PLANE('',#5980);
#734=PLANE('',#5984);
#735=PLANE('',#5985);
#736=PLANE('',#5990);
#737=PLANE('',#5994);
#738=PLANE('',#5995);
#739=PLANE('',#6001);
#740=PLANE('',#6002);
#741=PLANE('',#6004);
#742=PLANE('',#6010);
#743=PLANE('',#6015);
#744=PLANE('',#6017);
#745=PLANE('',#6019);
#746=PLANE('',#6025);
#747=PLANE('',#6026);
#748=PLANE('',#6032);
#749=PLANE('',#6034);
#750=PLANE('',#6035);
#751=PLANE('',#6036);
#752=PLANE('',#6040);
#753=PLANE('',#6053);
#754=PLANE('',#6055);
#755=PLANE('',#6059);
#756=PLANE('',#6064);
#757=PLANE('',#6080);
#758=PLANE('',#6211);
#759=PLANE('',#6346);
#760=PLANE('',#6349);
#761=PLANE('',#6352);
#762=PLANE('',#6356);
#763=PLANE('',#6359);
#764=PLANE('',#6370);
#765=PLANE('',#6371);
#766=PLANE('',#6373);
#767=PLANE('',#6387);
#768=PLANE('',#6388);
#769=PLANE('',#6401);
#770=PLANE('',#6406);
#771=PLANE('',#6412);
#772=PLANE('',#6414);
#773=PLANE('',#6421);
#774=PLANE('',#6432);
#775=PLANE('',#6438);
#776=PLANE('',#6451);
#777=PLANE('',#6459);
#778=PLANE('',#6469);
#779=PLANE('',#6471);
#780=PLANE('',#6472);
#781=PLANE('',#6474);
#782=PLANE('',#6477);
#783=PLANE('',#6480);
#784=PLANE('',#6488);
#785=PLANE('',#6490);
#786=PLANE('',#6496);
#787=PLANE('',#6500);
#788=PLANE('',#6501);
#789=PLANE('',#6502);
#790=B_SPLINE_CURVE_WITH_KNOTS('',3,(#8397,#8398,#8399,#8400,#8401,#8402,
#8403,#8404,#8405,#8406,#8407),.UNSPECIFIED.,.T.,.F.,(1,1,1,1,1,1,1,1,1,
1,1,1,1,1,1),(-0.0117279316645703,-0.00781862110971355,-0.00390931055485677,
0.,0.00390931055485677,0.00781862110971355,0.0117279316645703,0.0156372422194271,
0.0195465527742839,0.0234558633291406,0.0273651738839974,0.0312744844388542,
0.035183794993711,0.0390931055485677,0.0430024161034245),.UNSPECIFIED.);
#791=B_SPLINE_CURVE_WITH_KNOTS('',3,(#8414,#8415,#8416,#8417,#8418,#8419,
#8420,#8421,#8422,#8423,#8424),.UNSPECIFIED.,.T.,.F.,(1,1,1,1,1,1,1,1,1,
1,1,1,1,1,1),(-0.0117277673344821,-0.00781851155632137,-0.00390925577816069,
0.,0.00390925577816069,0.00781851155632137,0.0117277673344821,0.0156370231126427,
0.0195462788908034,0.0234555346689641,0.0273647904471248,0.0312740462252855,
0.0351833020034462,0.0390925577816069,0.0430018135597676),.UNSPECIFIED.);
#792=B_SPLINE_CURVE_WITH_KNOTS('',3,(#8466,#8467,#8468,#8469),
 .UNSPECIFIED.,.F.,.F.,(4,4),(0.000582701576065907,0.000731093758582388),
 .UNSPECIFIED.);
#793=B_SPLINE_CURVE_WITH_KNOTS('',3,(#8473,#8474,#8475,#8476),
 .UNSPECIFIED.,.F.,.F.,(4,4),(0.000110312006623771,0.000258881093106313),
 .UNSPECIFIED.);
#794=B_SPLINE_CURVE_WITH_KNOTS('',3,(#8491,#8492,#8493,#8494),
 .UNSPECIFIED.,.F.,.F.,(4,4),(0.00363875425759936,0.00424984212477264),
 .UNSPECIFIED.);
#795=B_SPLINE_CURVE_WITH_KNOTS('',3,(#8498,#8499,#8500,#8501),
 .UNSPECIFIED.,.F.,.F.,(4,4),(0.00363875425759936,0.00424984212477264),
 .UNSPECIFIED.);
#796=B_SPLINE_CURVE_WITH_KNOTS('',3,(#8502,#8503,#8504,#8505),
 .UNSPECIFIED.,.F.,.F.,(4,4),(0.00356470722087229,0.00417579509082418),
 .UNSPECIFIED.);
#797=B_SPLINE_CURVE_WITH_KNOTS('',3,(#8509,#8510,#8511,#8512),
 .UNSPECIFIED.,.F.,.F.,(4,4),(0.00356470722087229,0.00417579509082374),
 .UNSPECIFIED.);
#798=B_SPLINE_CURVE_WITH_KNOTS('',3,(#8520,#8521,#8522,#8523),
 .UNSPECIFIED.,.F.,.F.,(4,4),(0.000582701576065907,0.000731093758582387),
 .UNSPECIFIED.);
#799=B_SPLINE_CURVE_WITH_KNOTS('',3,(#8524,#8525,#8526,#8527),
 .UNSPECIFIED.,.F.,.F.,(4,4),(0.000110312006623771,0.000258881093106891),
 .UNSPECIFIED.);
#800=B_SPLINE_CURVE_WITH_KNOTS('',3,(#8971,#8972,#8973,#8974,#8975),
 .UNSPECIFIED.,.F.,.F.,(4,1,4),(0.,0.00143909544014382,0.00287819088028765),
 .UNSPECIFIED.);
#801=B_SPLINE_CURVE_WITH_KNOTS('',3,(#8993,#8994,#8995,#8996,#8997),
 .UNSPECIFIED.,.F.,.F.,(4,1,4),(0.,0.00143909544014381,0.00287819088028763),
 .UNSPECIFIED.);
#802=B_SPLINE_CURVE_WITH_KNOTS('',3,(#9833,#9834,#9835,#9836,#9837,#9838,
#9839),.UNSPECIFIED.,.F.,.F.,(4,1,1,1,4),(0.00864227471880883,0.00981748688955518,
0.0109926990603015,0.0121679112310479,0.0133431234017942),.UNSPECIFIED.);
#803=B_SPLINE_CURVE_WITH_KNOTS('',3,(#9853,#9854,#9855,#9856,#9857,#9858,
#9859),.UNSPECIFIED.,.F.,.F.,(4,1,1,1,4),(0.00546378704703531,0.00663876072579679,
0.00781373440455828,0.00898870808331976,0.0101636817620812),
 .UNSPECIFIED.);
#804=B_SPLINE_CURVE_WITH_KNOTS('',3,(#9864,#9865,#9866,#9867,#9868,#9869,
#9870),.UNSPECIFIED.,.F.,.F.,(4,1,1,1,4),(0.0142365147475521,0.0161947978067127,
0.0181530808658734,0.020111363925034,0.0220696469841946),.UNSPECIFIED.);
#805=B_SPLINE_CURVE_WITH_KNOTS('',3,(#9875,#9876,#9877,#9878,#9879,#9880,
#9881),.UNSPECIFIED.,.F.,.F.,(4,1,1,1,4),(0.00927377643444575,0.0112324591922964,
0.0131911419501471,0.0151498247079977,0.0171085074658484),.UNSPECIFIED.);
#806=B_SPLINE_CURVE_WITH_KNOTS('',3,(#10072,#10073,#10074,#10075),
 .UNSPECIFIED.,.F.,.F.,(4,4),(0.000582701576065907,0.000731093758582388),
 .UNSPECIFIED.);
#807=B_SPLINE_CURVE_WITH_KNOTS('',3,(#10079,#10080,#10081,#10082),
 .UNSPECIFIED.,.F.,.F.,(4,4),(0.000110312006623771,0.000258881093106313),
 .UNSPECIFIED.);
#808=B_SPLINE_CURVE_WITH_KNOTS('',3,(#10097,#10098,#10099,#10100),
 .UNSPECIFIED.,.F.,.F.,(4,4),(0.00363875425759936,0.00424984212477264),
 .UNSPECIFIED.);
#809=B_SPLINE_CURVE_WITH_KNOTS('',3,(#10104,#10105,#10106,#10107),
 .UNSPECIFIED.,.F.,.F.,(4,4),(0.00363875425759936,0.00424984212477264),
 .UNSPECIFIED.);
#810=B_SPLINE_CURVE_WITH_KNOTS('',3,(#10108,#10109,#10110,#10111),
 .UNSPECIFIED.,.F.,.F.,(4,4),(0.00356470722087229,0.00417579509082418),
 .UNSPECIFIED.);
#811=B_SPLINE_CURVE_WITH_KNOTS('',3,(#10115,#10116,#10117,#10118),
 .UNSPECIFIED.,.F.,.F.,(4,4),(0.00356470722087229,0.00417579509082374),
 .UNSPECIFIED.);
#812=B_SPLINE_CURVE_WITH_KNOTS('',3,(#10126,#10127,#10128,#10129),
 .UNSPECIFIED.,.F.,.F.,(4,4),(0.000582701576065907,0.000731093758582387),
 .UNSPECIFIED.);
#813=B_SPLINE_CURVE_WITH_KNOTS('',3,(#10130,#10131,#10132,#10133),
 .UNSPECIFIED.,.F.,.F.,(4,4),(0.000110312006623771,0.000258881093106891),
 .UNSPECIFIED.);
#814=ORIENTED_EDGE('',*,*,#2344,.T.);
#815=ORIENTED_EDGE('',*,*,#2345,.T.);
#816=ORIENTED_EDGE('',*,*,#2346,.T.);
#817=ORIENTED_EDGE('',*,*,#2347,.T.);
#818=ORIENTED_EDGE('',*,*,#2348,.F.);
#819=ORIENTED_EDGE('',*,*,#2349,.F.);
#820=ORIENTED_EDGE('',*,*,#2345,.F.);
#821=ORIENTED_EDGE('',*,*,#2350,.T.);
#822=ORIENTED_EDGE('',*,*,#2351,.T.);
#823=ORIENTED_EDGE('',*,*,#2352,.T.);
#824=ORIENTED_EDGE('',*,*,#2353,.T.);
#825=ORIENTED_EDGE('',*,*,#2354,.T.);
#826=ORIENTED_EDGE('',*,*,#2347,.F.);
#827=ORIENTED_EDGE('',*,*,#2355,.T.);
#828=ORIENTED_EDGE('',*,*,#2350,.F.);
#829=ORIENTED_EDGE('',*,*,#2348,.T.);
#830=ORIENTED_EDGE('',*,*,#2355,.F.);
#831=ORIENTED_EDGE('',*,*,#2356,.T.);
#832=ORIENTED_EDGE('',*,*,#2357,.T.);
#833=ORIENTED_EDGE('',*,*,#2358,.T.);
#834=ORIENTED_EDGE('',*,*,#2359,.T.);
#835=ORIENTED_EDGE('',*,*,#2344,.F.);
#836=ORIENTED_EDGE('',*,*,#2346,.F.);
#837=ORIENTED_EDGE('',*,*,#2349,.T.);
#838=ORIENTED_EDGE('',*,*,#2359,.F.);
#839=ORIENTED_EDGE('',*,*,#2354,.F.);
#840=ORIENTED_EDGE('',*,*,#2358,.F.);
#841=ORIENTED_EDGE('',*,*,#2353,.F.);
#842=ORIENTED_EDGE('',*,*,#2357,.F.);
#843=ORIENTED_EDGE('',*,*,#2352,.F.);
#844=ORIENTED_EDGE('',*,*,#2356,.F.);
#845=ORIENTED_EDGE('',*,*,#2351,.F.);
#846=ORIENTED_EDGE('',*,*,#2360,.F.);
#847=ORIENTED_EDGE('',*,*,#2361,.T.);
#848=ORIENTED_EDGE('',*,*,#2362,.F.);
#849=ORIENTED_EDGE('',*,*,#2363,.T.);
#850=ORIENTED_EDGE('',*,*,#2364,.F.);
#851=ORIENTED_EDGE('',*,*,#2365,.T.);
#852=ORIENTED_EDGE('',*,*,#2366,.T.);
#853=ORIENTED_EDGE('',*,*,#2367,.T.);
#854=ORIENTED_EDGE('',*,*,#2368,.T.);
#855=ORIENTED_EDGE('',*,*,#2364,.T.);
#856=ORIENTED_EDGE('',*,*,#2369,.T.);
#857=ORIENTED_EDGE('',*,*,#2370,.T.);
#858=ORIENTED_EDGE('',*,*,#2371,.T.);
#859=ORIENTED_EDGE('',*,*,#2372,.F.);
#860=ORIENTED_EDGE('',*,*,#2373,.F.);
#861=ORIENTED_EDGE('',*,*,#2362,.T.);
#862=ORIENTED_EDGE('',*,*,#2374,.F.);
#863=ORIENTED_EDGE('',*,*,#2375,.F.);
#864=ORIENTED_EDGE('',*,*,#2376,.T.);
#865=ORIENTED_EDGE('',*,*,#2377,.F.);
#866=ORIENTED_EDGE('',*,*,#2378,.F.);
#867=ORIENTED_EDGE('',*,*,#2377,.T.);
#868=ORIENTED_EDGE('',*,*,#2378,.T.);
#869=ORIENTED_EDGE('',*,*,#2367,.F.);
#870=ORIENTED_EDGE('',*,*,#2379,.F.);
#871=ORIENTED_EDGE('',*,*,#2370,.F.);
#872=ORIENTED_EDGE('',*,*,#2380,.F.);
#873=ORIENTED_EDGE('',*,*,#2361,.F.);
#874=ORIENTED_EDGE('',*,*,#2372,.T.);
#875=ORIENTED_EDGE('',*,*,#2381,.T.);
#876=ORIENTED_EDGE('',*,*,#2375,.T.);
#877=ORIENTED_EDGE('',*,*,#2382,.F.);
#878=ORIENTED_EDGE('',*,*,#2379,.T.);
#879=ORIENTED_EDGE('',*,*,#2360,.T.);
#880=ORIENTED_EDGE('',*,*,#2380,.T.);
#881=ORIENTED_EDGE('',*,*,#2376,.F.);
#882=ORIENTED_EDGE('',*,*,#2381,.F.);
#883=ORIENTED_EDGE('',*,*,#2371,.F.);
#884=ORIENTED_EDGE('',*,*,#2373,.T.);
#885=ORIENTED_EDGE('',*,*,#2382,.T.);
#886=ORIENTED_EDGE('',*,*,#2374,.T.);
#887=ORIENTED_EDGE('',*,*,#2365,.F.);
#888=ORIENTED_EDGE('',*,*,#2369,.F.);
#889=ORIENTED_EDGE('',*,*,#2363,.F.);
#890=ORIENTED_EDGE('',*,*,#2366,.F.);
#891=ORIENTED_EDGE('',*,*,#2368,.F.);
#892=ORIENTED_EDGE('',*,*,#2383,.T.);
#893=ORIENTED_EDGE('',*,*,#2384,.F.);
#894=ORIENTED_EDGE('',*,*,#2385,.F.);
#895=ORIENTED_EDGE('',*,*,#2386,.T.);
#896=ORIENTED_EDGE('',*,*,#2387,.F.);
#897=ORIENTED_EDGE('',*,*,#2388,.F.);
#898=ORIENTED_EDGE('',*,*,#2389,.T.);
#899=ORIENTED_EDGE('',*,*,#2390,.F.);
#900=ORIENTED_EDGE('',*,*,#2391,.F.);
#901=ORIENTED_EDGE('',*,*,#2392,.T.);
#902=ORIENTED_EDGE('',*,*,#2392,.F.);
#903=ORIENTED_EDGE('',*,*,#2393,.F.);
#904=ORIENTED_EDGE('',*,*,#2394,.F.);
#905=ORIENTED_EDGE('',*,*,#2395,.F.);
#906=ORIENTED_EDGE('',*,*,#2396,.F.);
#907=ORIENTED_EDGE('',*,*,#2385,.T.);
#908=ORIENTED_EDGE('',*,*,#2397,.F.);
#909=ORIENTED_EDGE('',*,*,#2398,.F.);
#910=ORIENTED_EDGE('',*,*,#2399,.F.);
#911=ORIENTED_EDGE('',*,*,#2400,.T.);
#912=ORIENTED_EDGE('',*,*,#2401,.F.);
#913=ORIENTED_EDGE('',*,*,#2402,.F.);
#914=ORIENTED_EDGE('',*,*,#2403,.F.);
#915=ORIENTED_EDGE('',*,*,#2404,.T.);
#916=ORIENTED_EDGE('',*,*,#2405,.F.);
#917=ORIENTED_EDGE('',*,*,#2406,.F.);
#918=ORIENTED_EDGE('',*,*,#2407,.F.);
#919=ORIENTED_EDGE('',*,*,#2408,.T.);
#920=ORIENTED_EDGE('',*,*,#2409,.F.);
#921=ORIENTED_EDGE('',*,*,#2410,.F.);
#922=ORIENTED_EDGE('',*,*,#2411,.F.);
#923=ORIENTED_EDGE('',*,*,#2412,.T.);
#924=ORIENTED_EDGE('',*,*,#2413,.F.);
#925=ORIENTED_EDGE('',*,*,#2414,.F.);
#926=ORIENTED_EDGE('',*,*,#2415,.F.);
#927=ORIENTED_EDGE('',*,*,#2416,.T.);
#928=ORIENTED_EDGE('',*,*,#2417,.F.);
#929=ORIENTED_EDGE('',*,*,#2418,.F.);
#930=ORIENTED_EDGE('',*,*,#2419,.F.);
#931=ORIENTED_EDGE('',*,*,#2420,.T.);
#932=ORIENTED_EDGE('',*,*,#2421,.F.);
#933=ORIENTED_EDGE('',*,*,#2422,.F.);
#934=ORIENTED_EDGE('',*,*,#2423,.F.);
#935=ORIENTED_EDGE('',*,*,#2424,.T.);
#936=ORIENTED_EDGE('',*,*,#2425,.F.);
#937=ORIENTED_EDGE('',*,*,#2426,.F.);
#938=ORIENTED_EDGE('',*,*,#2427,.F.);
#939=ORIENTED_EDGE('',*,*,#2428,.T.);
#940=ORIENTED_EDGE('',*,*,#2429,.F.);
#941=ORIENTED_EDGE('',*,*,#2430,.F.);
#942=ORIENTED_EDGE('',*,*,#2431,.F.);
#943=ORIENTED_EDGE('',*,*,#2432,.T.);
#944=ORIENTED_EDGE('',*,*,#2433,.F.);
#945=ORIENTED_EDGE('',*,*,#2434,.F.);
#946=ORIENTED_EDGE('',*,*,#2435,.F.);
#947=ORIENTED_EDGE('',*,*,#2436,.T.);
#948=ORIENTED_EDGE('',*,*,#2437,.F.);
#949=ORIENTED_EDGE('',*,*,#2438,.F.);
#950=ORIENTED_EDGE('',*,*,#2439,.F.);
#951=ORIENTED_EDGE('',*,*,#2387,.T.);
#952=ORIENTED_EDGE('',*,*,#2440,.T.);
#953=ORIENTED_EDGE('',*,*,#2441,.T.);
#954=ORIENTED_EDGE('',*,*,#2442,.T.);
#955=ORIENTED_EDGE('',*,*,#2443,.T.);
#956=ORIENTED_EDGE('',*,*,#2444,.T.);
#957=ORIENTED_EDGE('',*,*,#2445,.T.);
#958=ORIENTED_EDGE('',*,*,#2446,.T.);
#959=ORIENTED_EDGE('',*,*,#2391,.T.);
#960=ORIENTED_EDGE('',*,*,#2447,.F.);
#961=ORIENTED_EDGE('',*,*,#2383,.F.);
#962=ORIENTED_EDGE('',*,*,#2448,.F.);
#963=ORIENTED_EDGE('',*,*,#2449,.F.);
#964=ORIENTED_EDGE('',*,*,#2450,.F.);
#965=ORIENTED_EDGE('',*,*,#2451,.F.);
#966=ORIENTED_EDGE('',*,*,#2452,.F.);
#967=ORIENTED_EDGE('',*,*,#2453,.F.);
#968=ORIENTED_EDGE('',*,*,#2454,.F.);
#969=ORIENTED_EDGE('',*,*,#2389,.F.);
#970=ORIENTED_EDGE('',*,*,#2455,.F.);
#971=ORIENTED_EDGE('',*,*,#2456,.F.);
#972=ORIENTED_EDGE('',*,*,#2457,.F.);
#973=ORIENTED_EDGE('',*,*,#2458,.F.);
#974=ORIENTED_EDGE('',*,*,#2459,.F.);
#975=ORIENTED_EDGE('',*,*,#2460,.F.);
#976=ORIENTED_EDGE('',*,*,#2461,.F.);
#977=ORIENTED_EDGE('',*,*,#2462,.F.);
#978=ORIENTED_EDGE('',*,*,#2463,.F.);
#979=ORIENTED_EDGE('',*,*,#2464,.F.);
#980=ORIENTED_EDGE('',*,*,#2465,.F.);
#981=ORIENTED_EDGE('',*,*,#2466,.F.);
#982=ORIENTED_EDGE('',*,*,#2467,.F.);
#983=ORIENTED_EDGE('',*,*,#2468,.F.);
#984=ORIENTED_EDGE('',*,*,#2469,.F.);
#985=ORIENTED_EDGE('',*,*,#2470,.F.);
#986=ORIENTED_EDGE('',*,*,#2471,.F.);
#987=ORIENTED_EDGE('',*,*,#2472,.F.);
#988=ORIENTED_EDGE('',*,*,#2473,.F.);
#989=ORIENTED_EDGE('',*,*,#2474,.F.);
#990=ORIENTED_EDGE('',*,*,#2475,.F.);
#991=ORIENTED_EDGE('',*,*,#2476,.F.);
#992=ORIENTED_EDGE('',*,*,#2477,.F.);
#993=ORIENTED_EDGE('',*,*,#2478,.F.);
#994=ORIENTED_EDGE('',*,*,#2479,.F.);
#995=ORIENTED_EDGE('',*,*,#2480,.F.);
#996=ORIENTED_EDGE('',*,*,#2481,.F.);
#997=ORIENTED_EDGE('',*,*,#2482,.F.);
#998=ORIENTED_EDGE('',*,*,#2483,.F.);
#999=ORIENTED_EDGE('',*,*,#2484,.F.);
#1000=ORIENTED_EDGE('',*,*,#2485,.F.);
#1001=ORIENTED_EDGE('',*,*,#2486,.F.);
#1002=ORIENTED_EDGE('',*,*,#2487,.F.);
#1003=ORIENTED_EDGE('',*,*,#2488,.F.);
#1004=ORIENTED_EDGE('',*,*,#2489,.F.);
#1005=ORIENTED_EDGE('',*,*,#2490,.F.);
#1006=ORIENTED_EDGE('',*,*,#2491,.F.);
#1007=ORIENTED_EDGE('',*,*,#2492,.F.);
#1008=ORIENTED_EDGE('',*,*,#2493,.F.);
#1009=ORIENTED_EDGE('',*,*,#2494,.F.);
#1010=ORIENTED_EDGE('',*,*,#2495,.F.);
#1011=ORIENTED_EDGE('',*,*,#2496,.F.);
#1012=ORIENTED_EDGE('',*,*,#2497,.T.);
#1013=ORIENTED_EDGE('',*,*,#2498,.T.);
#1014=ORIENTED_EDGE('',*,*,#2499,.T.);
#1015=ORIENTED_EDGE('',*,*,#2500,.T.);
#1016=ORIENTED_EDGE('',*,*,#2454,.T.);
#1017=ORIENTED_EDGE('',*,*,#2501,.F.);
#1018=ORIENTED_EDGE('',*,*,#2440,.F.);
#1019=ORIENTED_EDGE('',*,*,#2390,.T.);
#1020=ORIENTED_EDGE('',*,*,#2448,.T.);
#1021=ORIENTED_EDGE('',*,*,#2386,.F.);
#1022=ORIENTED_EDGE('',*,*,#2446,.F.);
#1023=ORIENTED_EDGE('',*,*,#2502,.T.);
#1024=ORIENTED_EDGE('',*,*,#2449,.T.);
#1025=ORIENTED_EDGE('',*,*,#2502,.F.);
#1026=ORIENTED_EDGE('',*,*,#2445,.F.);
#1027=ORIENTED_EDGE('',*,*,#2503,.T.);
#1028=ORIENTED_EDGE('',*,*,#2450,.T.);
#1029=ORIENTED_EDGE('',*,*,#2503,.F.);
#1030=ORIENTED_EDGE('',*,*,#2444,.F.);
#1031=ORIENTED_EDGE('',*,*,#2504,.T.);
#1032=ORIENTED_EDGE('',*,*,#2451,.T.);
#1033=ORIENTED_EDGE('',*,*,#2504,.F.);
#1034=ORIENTED_EDGE('',*,*,#2443,.F.);
#1035=ORIENTED_EDGE('',*,*,#2505,.T.);
#1036=ORIENTED_EDGE('',*,*,#2452,.T.);
#1037=ORIENTED_EDGE('',*,*,#2505,.F.);
#1038=ORIENTED_EDGE('',*,*,#2442,.F.);
#1039=ORIENTED_EDGE('',*,*,#2506,.T.);
#1040=ORIENTED_EDGE('',*,*,#2453,.T.);
#1041=ORIENTED_EDGE('',*,*,#2506,.F.);
#1042=ORIENTED_EDGE('',*,*,#2441,.F.);
#1043=ORIENTED_EDGE('',*,*,#2501,.T.);
#1044=ORIENTED_EDGE('',*,*,#2497,.F.);
#1045=ORIENTED_EDGE('',*,*,#2507,.F.);
#1046=ORIENTED_EDGE('',*,*,#2394,.T.);
#1047=ORIENTED_EDGE('',*,*,#2508,.T.);
#1048=ORIENTED_EDGE('',*,*,#2498,.F.);
#1049=ORIENTED_EDGE('',*,*,#2508,.F.);
#1050=ORIENTED_EDGE('',*,*,#2393,.T.);
#1051=ORIENTED_EDGE('',*,*,#2509,.T.);
#1052=ORIENTED_EDGE('',*,*,#2499,.F.);
#1053=ORIENTED_EDGE('',*,*,#2509,.F.);
#1054=ORIENTED_EDGE('',*,*,#2396,.T.);
#1055=ORIENTED_EDGE('',*,*,#2510,.T.);
#1056=ORIENTED_EDGE('',*,*,#2500,.F.);
#1057=ORIENTED_EDGE('',*,*,#2510,.F.);
#1058=ORIENTED_EDGE('',*,*,#2395,.T.);
#1059=ORIENTED_EDGE('',*,*,#2507,.T.);
#1060=ORIENTED_EDGE('',*,*,#2511,.F.);
#1061=ORIENTED_EDGE('',*,*,#2458,.T.);
#1062=ORIENTED_EDGE('',*,*,#2512,.F.);
#1063=ORIENTED_EDGE('',*,*,#2436,.F.);
#1064=ORIENTED_EDGE('',*,*,#2513,.F.);
#1065=ORIENTED_EDGE('',*,*,#2462,.T.);
#1066=ORIENTED_EDGE('',*,*,#2514,.F.);
#1067=ORIENTED_EDGE('',*,*,#2432,.F.);
#1068=ORIENTED_EDGE('',*,*,#2515,.F.);
#1069=ORIENTED_EDGE('',*,*,#2428,.F.);
#1070=ORIENTED_EDGE('',*,*,#2516,.F.);
#1071=ORIENTED_EDGE('',*,*,#2466,.T.);
#1072=ORIENTED_EDGE('',*,*,#2517,.F.);
#1073=ORIENTED_EDGE('',*,*,#2424,.F.);
#1074=ORIENTED_EDGE('',*,*,#2518,.F.);
#1075=ORIENTED_EDGE('',*,*,#2470,.T.);
#1076=ORIENTED_EDGE('',*,*,#2519,.F.);
#1077=ORIENTED_EDGE('',*,*,#2474,.T.);
#1078=ORIENTED_EDGE('',*,*,#2520,.F.);
#1079=ORIENTED_EDGE('',*,*,#2420,.F.);
#1080=ORIENTED_EDGE('',*,*,#2521,.F.);
#1081=ORIENTED_EDGE('',*,*,#2478,.T.);
#1082=ORIENTED_EDGE('',*,*,#2522,.F.);
#1083=ORIENTED_EDGE('',*,*,#2416,.F.);
#1084=ORIENTED_EDGE('',*,*,#2523,.F.);
#1085=ORIENTED_EDGE('',*,*,#2412,.F.);
#1086=ORIENTED_EDGE('',*,*,#2524,.F.);
#1087=ORIENTED_EDGE('',*,*,#2482,.T.);
#1088=ORIENTED_EDGE('',*,*,#2525,.F.);
#1089=ORIENTED_EDGE('',*,*,#2486,.T.);
#1090=ORIENTED_EDGE('',*,*,#2526,.F.);
#1091=ORIENTED_EDGE('',*,*,#2408,.F.);
#1092=ORIENTED_EDGE('',*,*,#2527,.F.);
#1093=ORIENTED_EDGE('',*,*,#2490,.T.);
#1094=ORIENTED_EDGE('',*,*,#2528,.F.);
#1095=ORIENTED_EDGE('',*,*,#2404,.F.);
#1096=ORIENTED_EDGE('',*,*,#2529,.F.);
#1097=ORIENTED_EDGE('',*,*,#2494,.T.);
#1098=ORIENTED_EDGE('',*,*,#2530,.F.);
#1099=ORIENTED_EDGE('',*,*,#2400,.F.);
#1100=ORIENTED_EDGE('',*,*,#2384,.T.);
#1101=ORIENTED_EDGE('',*,*,#2447,.T.);
#1102=ORIENTED_EDGE('',*,*,#2531,.F.);
#1103=ORIENTED_EDGE('',*,*,#2397,.T.);
#1104=ORIENTED_EDGE('',*,*,#2531,.T.);
#1105=ORIENTED_EDGE('',*,*,#2496,.T.);
#1106=ORIENTED_EDGE('',*,*,#2532,.F.);
#1107=ORIENTED_EDGE('',*,*,#2398,.T.);
#1108=ORIENTED_EDGE('',*,*,#2532,.T.);
#1109=ORIENTED_EDGE('',*,*,#2495,.T.);
#1110=ORIENTED_EDGE('',*,*,#2529,.T.);
#1111=ORIENTED_EDGE('',*,*,#2399,.T.);
#1112=ORIENTED_EDGE('',*,*,#2530,.T.);
#1113=ORIENTED_EDGE('',*,*,#2493,.T.);
#1114=ORIENTED_EDGE('',*,*,#2533,.F.);
#1115=ORIENTED_EDGE('',*,*,#2401,.T.);
#1116=ORIENTED_EDGE('',*,*,#2533,.T.);
#1117=ORIENTED_EDGE('',*,*,#2492,.T.);
#1118=ORIENTED_EDGE('',*,*,#2534,.F.);
#1119=ORIENTED_EDGE('',*,*,#2402,.T.);
#1120=ORIENTED_EDGE('',*,*,#2534,.T.);
#1121=ORIENTED_EDGE('',*,*,#2491,.T.);
#1122=ORIENTED_EDGE('',*,*,#2527,.T.);
#1123=ORIENTED_EDGE('',*,*,#2403,.T.);
#1124=ORIENTED_EDGE('',*,*,#2528,.T.);
#1125=ORIENTED_EDGE('',*,*,#2489,.T.);
#1126=ORIENTED_EDGE('',*,*,#2535,.F.);
#1127=ORIENTED_EDGE('',*,*,#2405,.T.);
#1128=ORIENTED_EDGE('',*,*,#2535,.T.);
#1129=ORIENTED_EDGE('',*,*,#2488,.T.);
#1130=ORIENTED_EDGE('',*,*,#2536,.F.);
#1131=ORIENTED_EDGE('',*,*,#2406,.T.);
#1132=ORIENTED_EDGE('',*,*,#2536,.T.);
#1133=ORIENTED_EDGE('',*,*,#2487,.T.);
#1134=ORIENTED_EDGE('',*,*,#2525,.T.);
#1135=ORIENTED_EDGE('',*,*,#2407,.T.);
#1136=ORIENTED_EDGE('',*,*,#2526,.T.);
#1137=ORIENTED_EDGE('',*,*,#2485,.T.);
#1138=ORIENTED_EDGE('',*,*,#2537,.F.);
#1139=ORIENTED_EDGE('',*,*,#2409,.T.);
#1140=ORIENTED_EDGE('',*,*,#2537,.T.);
#1141=ORIENTED_EDGE('',*,*,#2484,.T.);
#1142=ORIENTED_EDGE('',*,*,#2538,.F.);
#1143=ORIENTED_EDGE('',*,*,#2410,.T.);
#1144=ORIENTED_EDGE('',*,*,#2538,.T.);
#1145=ORIENTED_EDGE('',*,*,#2483,.T.);
#1146=ORIENTED_EDGE('',*,*,#2524,.T.);
#1147=ORIENTED_EDGE('',*,*,#2411,.T.);
#1148=ORIENTED_EDGE('',*,*,#2523,.T.);
#1149=ORIENTED_EDGE('',*,*,#2481,.T.);
#1150=ORIENTED_EDGE('',*,*,#2539,.F.);
#1151=ORIENTED_EDGE('',*,*,#2413,.T.);
#1152=ORIENTED_EDGE('',*,*,#2539,.T.);
#1153=ORIENTED_EDGE('',*,*,#2480,.T.);
#1154=ORIENTED_EDGE('',*,*,#2540,.F.);
#1155=ORIENTED_EDGE('',*,*,#2414,.T.);
#1156=ORIENTED_EDGE('',*,*,#2540,.T.);
#1157=ORIENTED_EDGE('',*,*,#2479,.T.);
#1158=ORIENTED_EDGE('',*,*,#2521,.T.);
#1159=ORIENTED_EDGE('',*,*,#2415,.T.);
#1160=ORIENTED_EDGE('',*,*,#2522,.T.);
#1161=ORIENTED_EDGE('',*,*,#2477,.T.);
#1162=ORIENTED_EDGE('',*,*,#2541,.F.);
#1163=ORIENTED_EDGE('',*,*,#2417,.T.);
#1164=ORIENTED_EDGE('',*,*,#2541,.T.);
#1165=ORIENTED_EDGE('',*,*,#2476,.T.);
#1166=ORIENTED_EDGE('',*,*,#2542,.F.);
#1167=ORIENTED_EDGE('',*,*,#2418,.T.);
#1168=ORIENTED_EDGE('',*,*,#2542,.T.);
#1169=ORIENTED_EDGE('',*,*,#2475,.T.);
#1170=ORIENTED_EDGE('',*,*,#2519,.T.);
#1171=ORIENTED_EDGE('',*,*,#2419,.T.);
#1172=ORIENTED_EDGE('',*,*,#2520,.T.);
#1173=ORIENTED_EDGE('',*,*,#2473,.T.);
#1174=ORIENTED_EDGE('',*,*,#2543,.F.);
#1175=ORIENTED_EDGE('',*,*,#2421,.T.);
#1176=ORIENTED_EDGE('',*,*,#2543,.T.);
#1177=ORIENTED_EDGE('',*,*,#2472,.T.);
#1178=ORIENTED_EDGE('',*,*,#2544,.F.);
#1179=ORIENTED_EDGE('',*,*,#2422,.T.);
#1180=ORIENTED_EDGE('',*,*,#2544,.T.);
#1181=ORIENTED_EDGE('',*,*,#2471,.T.);
#1182=ORIENTED_EDGE('',*,*,#2518,.T.);
#1183=ORIENTED_EDGE('',*,*,#2423,.T.);
#1184=ORIENTED_EDGE('',*,*,#2517,.T.);
#1185=ORIENTED_EDGE('',*,*,#2469,.T.);
#1186=ORIENTED_EDGE('',*,*,#2545,.F.);
#1187=ORIENTED_EDGE('',*,*,#2425,.T.);
#1188=ORIENTED_EDGE('',*,*,#2545,.T.);
#1189=ORIENTED_EDGE('',*,*,#2468,.T.);
#1190=ORIENTED_EDGE('',*,*,#2546,.F.);
#1191=ORIENTED_EDGE('',*,*,#2426,.T.);
#1192=ORIENTED_EDGE('',*,*,#2546,.T.);
#1193=ORIENTED_EDGE('',*,*,#2467,.T.);
#1194=ORIENTED_EDGE('',*,*,#2516,.T.);
#1195=ORIENTED_EDGE('',*,*,#2427,.T.);
#1196=ORIENTED_EDGE('',*,*,#2515,.T.);
#1197=ORIENTED_EDGE('',*,*,#2465,.T.);
#1198=ORIENTED_EDGE('',*,*,#2547,.F.);
#1199=ORIENTED_EDGE('',*,*,#2429,.T.);
#1200=ORIENTED_EDGE('',*,*,#2547,.T.);
#1201=ORIENTED_EDGE('',*,*,#2464,.T.);
#1202=ORIENTED_EDGE('',*,*,#2548,.F.);
#1203=ORIENTED_EDGE('',*,*,#2430,.T.);
#1204=ORIENTED_EDGE('',*,*,#2548,.T.);
#1205=ORIENTED_EDGE('',*,*,#2463,.T.);
#1206=ORIENTED_EDGE('',*,*,#2513,.T.);
#1207=ORIENTED_EDGE('',*,*,#2431,.T.);
#1208=ORIENTED_EDGE('',*,*,#2514,.T.);
#1209=ORIENTED_EDGE('',*,*,#2461,.T.);
#1210=ORIENTED_EDGE('',*,*,#2549,.F.);
#1211=ORIENTED_EDGE('',*,*,#2433,.T.);
#1212=ORIENTED_EDGE('',*,*,#2549,.T.);
#1213=ORIENTED_EDGE('',*,*,#2460,.T.);
#1214=ORIENTED_EDGE('',*,*,#2550,.F.);
#1215=ORIENTED_EDGE('',*,*,#2434,.T.);
#1216=ORIENTED_EDGE('',*,*,#2550,.T.);
#1217=ORIENTED_EDGE('',*,*,#2459,.T.);
#1218=ORIENTED_EDGE('',*,*,#2511,.T.);
#1219=ORIENTED_EDGE('',*,*,#2435,.T.);
#1220=ORIENTED_EDGE('',*,*,#2512,.T.);
#1221=ORIENTED_EDGE('',*,*,#2457,.T.);
#1222=ORIENTED_EDGE('',*,*,#2551,.F.);
#1223=ORIENTED_EDGE('',*,*,#2437,.T.);
#1224=ORIENTED_EDGE('',*,*,#2551,.T.);
#1225=ORIENTED_EDGE('',*,*,#2456,.T.);
#1226=ORIENTED_EDGE('',*,*,#2552,.F.);
#1227=ORIENTED_EDGE('',*,*,#2438,.T.);
#1228=ORIENTED_EDGE('',*,*,#2552,.T.);
#1229=ORIENTED_EDGE('',*,*,#2455,.T.);
#1230=ORIENTED_EDGE('',*,*,#2388,.T.);
#1231=ORIENTED_EDGE('',*,*,#2439,.T.);
#1232=ORIENTED_EDGE('',*,*,#2553,.T.);
#1233=ORIENTED_EDGE('',*,*,#2554,.T.);
#1234=ORIENTED_EDGE('',*,*,#2555,.T.);
#1235=ORIENTED_EDGE('',*,*,#2556,.F.);
#1236=ORIENTED_EDGE('',*,*,#2557,.T.);
#1237=ORIENTED_EDGE('',*,*,#2558,.T.);
#1238=ORIENTED_EDGE('',*,*,#2559,.T.);
#1239=ORIENTED_EDGE('',*,*,#2560,.T.);
#1240=ORIENTED_EDGE('',*,*,#2561,.T.);
#1241=ORIENTED_EDGE('',*,*,#2562,.F.);
#1242=ORIENTED_EDGE('',*,*,#2563,.T.);
#1243=ORIENTED_EDGE('',*,*,#2564,.F.);
#1244=ORIENTED_EDGE('',*,*,#2565,.F.);
#1245=ORIENTED_EDGE('',*,*,#2566,.F.);
#1246=ORIENTED_EDGE('',*,*,#2567,.T.);
#1247=ORIENTED_EDGE('',*,*,#2568,.F.);
#1248=ORIENTED_EDGE('',*,*,#2569,.T.);
#1249=ORIENTED_EDGE('',*,*,#2570,.F.);
#1250=ORIENTED_EDGE('',*,*,#2571,.F.);
#1251=ORIENTED_EDGE('',*,*,#2572,.T.);
#1252=ORIENTED_EDGE('',*,*,#2573,.F.);
#1253=ORIENTED_EDGE('',*,*,#2574,.T.);
#1254=ORIENTED_EDGE('',*,*,#2575,.T.);
#1255=ORIENTED_EDGE('',*,*,#2576,.T.);
#1256=ORIENTED_EDGE('',*,*,#2577,.F.);
#1257=ORIENTED_EDGE('',*,*,#2578,.T.);
#1258=ORIENTED_EDGE('',*,*,#2579,.F.);
#1259=ORIENTED_EDGE('',*,*,#2580,.F.);
#1260=ORIENTED_EDGE('',*,*,#2581,.T.);
#1261=ORIENTED_EDGE('',*,*,#2582,.T.);
#1262=ORIENTED_EDGE('',*,*,#2583,.T.);
#1263=ORIENTED_EDGE('',*,*,#2584,.T.);
#1264=ORIENTED_EDGE('',*,*,#2585,.F.);
#1265=ORIENTED_EDGE('',*,*,#2586,.T.);
#1266=ORIENTED_EDGE('',*,*,#2587,.T.);
#1267=ORIENTED_EDGE('',*,*,#2588,.T.);
#1268=ORIENTED_EDGE('',*,*,#2589,.T.);
#1269=ORIENTED_EDGE('',*,*,#2590,.T.);
#1270=ORIENTED_EDGE('',*,*,#2563,.F.);
#1271=ORIENTED_EDGE('',*,*,#2591,.T.);
#1272=ORIENTED_EDGE('',*,*,#2553,.F.);
#1273=ORIENTED_EDGE('',*,*,#2592,.F.);
#1274=ORIENTED_EDGE('',*,*,#2593,.F.);
#1275=ORIENTED_EDGE('',*,*,#2594,.F.);
#1276=ORIENTED_EDGE('',*,*,#2559,.F.);
#1277=ORIENTED_EDGE('',*,*,#2595,.T.);
#1278=ORIENTED_EDGE('',*,*,#2572,.F.);
#1279=ORIENTED_EDGE('',*,*,#2596,.F.);
#1280=ORIENTED_EDGE('',*,*,#2555,.F.);
#1281=ORIENTED_EDGE('',*,*,#2597,.T.);
#1282=ORIENTED_EDGE('',*,*,#2582,.F.);
#1283=ORIENTED_EDGE('',*,*,#2598,.F.);
#1284=ORIENTED_EDGE('',*,*,#2588,.F.);
#1285=ORIENTED_EDGE('',*,*,#2599,.T.);
#1286=ORIENTED_EDGE('',*,*,#2557,.F.);
#1287=ORIENTED_EDGE('',*,*,#2600,.F.);
#1288=ORIENTED_EDGE('',*,*,#2584,.F.);
#1289=ORIENTED_EDGE('',*,*,#2601,.T.);
#1290=ORIENTED_EDGE('',*,*,#2576,.F.);
#1291=ORIENTED_EDGE('',*,*,#2602,.F.);
#1292=ORIENTED_EDGE('',*,*,#2578,.F.);
#1293=ORIENTED_EDGE('',*,*,#2603,.T.);
#1294=ORIENTED_EDGE('',*,*,#2586,.F.);
#1295=ORIENTED_EDGE('',*,*,#2604,.F.);
#1296=ORIENTED_EDGE('',*,*,#2574,.F.);
#1297=ORIENTED_EDGE('',*,*,#2605,.T.);
#1298=ORIENTED_EDGE('',*,*,#2567,.F.);
#1299=ORIENTED_EDGE('',*,*,#2606,.F.);
#1300=ORIENTED_EDGE('',*,*,#2607,.F.);
#1301=ORIENTED_EDGE('',*,*,#2608,.F.);
#1302=ORIENTED_EDGE('',*,*,#2569,.F.);
#1303=ORIENTED_EDGE('',*,*,#2609,.T.);
#1304=ORIENTED_EDGE('',*,*,#2581,.F.);
#1305=ORIENTED_EDGE('',*,*,#2610,.F.);
#1306=ORIENTED_EDGE('',*,*,#2611,.T.);
#1307=ORIENTED_EDGE('',*,*,#2607,.T.);
#1308=ORIENTED_EDGE('',*,*,#2612,.F.);
#1309=ORIENTED_EDGE('',*,*,#2613,.F.);
#1310=ORIENTED_EDGE('',*,*,#2614,.F.);
#1311=ORIENTED_EDGE('',*,*,#2593,.T.);
#1312=ORIENTED_EDGE('',*,*,#2571,.T.);
#1313=ORIENTED_EDGE('',*,*,#2615,.T.);
#1314=ORIENTED_EDGE('',*,*,#2560,.F.);
#1315=ORIENTED_EDGE('',*,*,#2596,.T.);
#1316=ORIENTED_EDGE('',*,*,#2589,.F.);
#1317=ORIENTED_EDGE('',*,*,#2600,.T.);
#1318=ORIENTED_EDGE('',*,*,#2561,.F.);
#1319=ORIENTED_EDGE('',*,*,#2616,.T.);
#1320=ORIENTED_EDGE('',*,*,#2579,.T.);
#1321=ORIENTED_EDGE('',*,*,#2604,.T.);
#1322=ORIENTED_EDGE('',*,*,#2590,.F.);
#1323=ORIENTED_EDGE('',*,*,#2617,.T.);
#1324=ORIENTED_EDGE('',*,*,#2618,.T.);
#1325=ORIENTED_EDGE('',*,*,#2619,.F.);
#1326=ORIENTED_EDGE('',*,*,#2620,.F.);
#1327=ORIENTED_EDGE('',*,*,#2621,.T.);
#1328=ORIENTED_EDGE('',*,*,#2570,.T.);
#1329=ORIENTED_EDGE('',*,*,#2610,.T.);
#1330=ORIENTED_EDGE('',*,*,#2580,.T.);
#1331=ORIENTED_EDGE('',*,*,#2622,.T.);
#1332=ORIENTED_EDGE('',*,*,#2575,.F.);
#1333=ORIENTED_EDGE('',*,*,#2608,.T.);
#1334=ORIENTED_EDGE('',*,*,#2611,.F.);
#1335=ORIENTED_EDGE('',*,*,#2592,.T.);
#1336=ORIENTED_EDGE('',*,*,#2556,.T.);
#1337=ORIENTED_EDGE('',*,*,#2598,.T.);
#1338=ORIENTED_EDGE('',*,*,#2585,.T.);
#1339=ORIENTED_EDGE('',*,*,#2602,.T.);
#1340=ORIENTED_EDGE('',*,*,#2623,.T.);
#1341=ORIENTED_EDGE('',*,*,#2624,.T.);
#1342=ORIENTED_EDGE('',*,*,#2625,.F.);
#1343=ORIENTED_EDGE('',*,*,#2626,.T.);
#1344=ORIENTED_EDGE('',*,*,#2624,.F.);
#1345=ORIENTED_EDGE('',*,*,#2626,.F.);
#1346=ORIENTED_EDGE('',*,*,#2564,.T.);
#1347=ORIENTED_EDGE('',*,*,#2594,.T.);
#1348=ORIENTED_EDGE('',*,*,#2614,.T.);
#1349=ORIENTED_EDGE('',*,*,#2627,.F.);
#1350=ORIENTED_EDGE('',*,*,#2628,.F.);
#1351=ORIENTED_EDGE('',*,*,#2629,.T.);
#1352=ORIENTED_EDGE('',*,*,#2630,.F.);
#1353=ORIENTED_EDGE('',*,*,#2631,.T.);
#1354=ORIENTED_EDGE('',*,*,#2632,.F.);
#1355=ORIENTED_EDGE('',*,*,#2633,.T.);
#1356=ORIENTED_EDGE('',*,*,#2565,.T.);
#1357=ORIENTED_EDGE('',*,*,#2629,.F.);
#1358=ORIENTED_EDGE('',*,*,#2612,.T.);
#1359=ORIENTED_EDGE('',*,*,#2606,.T.);
#1360=ORIENTED_EDGE('',*,*,#2566,.T.);
#1361=ORIENTED_EDGE('',*,*,#2633,.F.);
#1362=ORIENTED_EDGE('',*,*,#2634,.F.);
#1363=ORIENTED_EDGE('',*,*,#2635,.T.);
#1364=ORIENTED_EDGE('',*,*,#2613,.T.);
#1365=ORIENTED_EDGE('',*,*,#2635,.F.);
#1366=ORIENTED_EDGE('',*,*,#2636,.F.);
#1367=ORIENTED_EDGE('',*,*,#2627,.T.);
#1368=ORIENTED_EDGE('',*,*,#2637,.F.);
#1369=ORIENTED_EDGE('',*,*,#2618,.F.);
#1370=ORIENTED_EDGE('',*,*,#2638,.F.);
#1371=ORIENTED_EDGE('',*,*,#2639,.F.);
#1372=ORIENTED_EDGE('',*,*,#2640,.F.);
#1373=ORIENTED_EDGE('',*,*,#2641,.F.);
#1374=ORIENTED_EDGE('',*,*,#2642,.F.);
#1375=ORIENTED_EDGE('',*,*,#2630,.T.);
#1376=ORIENTED_EDGE('',*,*,#2628,.T.);
#1377=ORIENTED_EDGE('',*,*,#2636,.T.);
#1378=ORIENTED_EDGE('',*,*,#2634,.T.);
#1379=ORIENTED_EDGE('',*,*,#2632,.T.);
#1380=ORIENTED_EDGE('',*,*,#2640,.T.);
#1381=ORIENTED_EDGE('',*,*,#2643,.F.);
#1382=ORIENTED_EDGE('',*,*,#2644,.F.);
#1383=ORIENTED_EDGE('',*,*,#2645,.T.);
#1384=ORIENTED_EDGE('',*,*,#2646,.F.);
#1385=ORIENTED_EDGE('',*,*,#2647,.F.);
#1386=ORIENTED_EDGE('',*,*,#2641,.T.);
#1387=ORIENTED_EDGE('',*,*,#2645,.F.);
#1388=ORIENTED_EDGE('',*,*,#2638,.T.);
#1389=ORIENTED_EDGE('',*,*,#2621,.F.);
#1390=ORIENTED_EDGE('',*,*,#2648,.F.);
#1391=ORIENTED_EDGE('',*,*,#2649,.T.);
#1392=ORIENTED_EDGE('',*,*,#2639,.T.);
#1393=ORIENTED_EDGE('',*,*,#2649,.F.);
#1394=ORIENTED_EDGE('',*,*,#2650,.F.);
#1395=ORIENTED_EDGE('',*,*,#2643,.T.);
#1396=ORIENTED_EDGE('',*,*,#2644,.T.);
#1397=ORIENTED_EDGE('',*,*,#2650,.T.);
#1398=ORIENTED_EDGE('',*,*,#2648,.T.);
#1399=ORIENTED_EDGE('',*,*,#2620,.T.);
#1400=ORIENTED_EDGE('',*,*,#2646,.T.);
#1401=ORIENTED_EDGE('',*,*,#2637,.T.);
#1402=ORIENTED_EDGE('',*,*,#2631,.F.);
#1403=ORIENTED_EDGE('',*,*,#2642,.T.);
#1404=ORIENTED_EDGE('',*,*,#2647,.T.);
#1405=ORIENTED_EDGE('',*,*,#2619,.T.);
#1406=ORIENTED_EDGE('',*,*,#2625,.T.);
#1407=ORIENTED_EDGE('',*,*,#2616,.F.);
#1408=ORIENTED_EDGE('',*,*,#2615,.F.);
#1409=ORIENTED_EDGE('',*,*,#2622,.F.);
#1410=ORIENTED_EDGE('',*,*,#2617,.F.);
#1411=ORIENTED_EDGE('',*,*,#2623,.F.);
#1412=ORIENTED_EDGE('',*,*,#2651,.T.);
#1413=ORIENTED_EDGE('',*,*,#2652,.F.);
#1414=ORIENTED_EDGE('',*,*,#2554,.F.);
#1415=ORIENTED_EDGE('',*,*,#2591,.F.);
#1416=ORIENTED_EDGE('',*,*,#2562,.T.);
#1417=ORIENTED_EDGE('',*,*,#2605,.F.);
#1418=ORIENTED_EDGE('',*,*,#2573,.T.);
#1419=ORIENTED_EDGE('',*,*,#2601,.F.);
#1420=ORIENTED_EDGE('',*,*,#2583,.F.);
#1421=ORIENTED_EDGE('',*,*,#2597,.F.);
#1422=ORIENTED_EDGE('',*,*,#2651,.F.);
#1423=ORIENTED_EDGE('',*,*,#2587,.F.);
#1424=ORIENTED_EDGE('',*,*,#2603,.F.);
#1425=ORIENTED_EDGE('',*,*,#2577,.T.);
#1426=ORIENTED_EDGE('',*,*,#2609,.F.);
#1427=ORIENTED_EDGE('',*,*,#2568,.T.);
#1428=ORIENTED_EDGE('',*,*,#2595,.F.);
#1429=ORIENTED_EDGE('',*,*,#2558,.F.);
#1430=ORIENTED_EDGE('',*,*,#2599,.F.);
#1431=ORIENTED_EDGE('',*,*,#2652,.T.);
#1432=ORIENTED_EDGE('',*,*,#2653,.F.);
#1433=ORIENTED_EDGE('',*,*,#2654,.F.);
#1434=ORIENTED_EDGE('',*,*,#2655,.T.);
#1435=ORIENTED_EDGE('',*,*,#2656,.T.);
#1436=ORIENTED_EDGE('',*,*,#2657,.T.);
#1437=ORIENTED_EDGE('',*,*,#2658,.T.);
#1438=ORIENTED_EDGE('',*,*,#2659,.F.);
#1439=ORIENTED_EDGE('',*,*,#2660,.F.);
#1440=ORIENTED_EDGE('',*,*,#2661,.F.);
#1441=ORIENTED_EDGE('',*,*,#2662,.F.);
#1442=ORIENTED_EDGE('',*,*,#2663,.F.);
#1443=ORIENTED_EDGE('',*,*,#2664,.T.);
#1444=ORIENTED_EDGE('',*,*,#2660,.T.);
#1445=ORIENTED_EDGE('',*,*,#2665,.F.);
#1446=ORIENTED_EDGE('',*,*,#2655,.F.);
#1447=ORIENTED_EDGE('',*,*,#2666,.T.);
#1448=ORIENTED_EDGE('',*,*,#2663,.T.);
#1449=ORIENTED_EDGE('',*,*,#2667,.F.);
#1450=ORIENTED_EDGE('',*,*,#2656,.F.);
#1451=ORIENTED_EDGE('',*,*,#2665,.T.);
#1452=ORIENTED_EDGE('',*,*,#2662,.T.);
#1453=ORIENTED_EDGE('',*,*,#2668,.F.);
#1454=ORIENTED_EDGE('',*,*,#2657,.F.);
#1455=ORIENTED_EDGE('',*,*,#2667,.T.);
#1456=ORIENTED_EDGE('',*,*,#2661,.T.);
#1457=ORIENTED_EDGE('',*,*,#2666,.F.);
#1458=ORIENTED_EDGE('',*,*,#2658,.F.);
#1459=ORIENTED_EDGE('',*,*,#2668,.T.);
#1460=ORIENTED_EDGE('',*,*,#2659,.T.);
#1461=ORIENTED_EDGE('',*,*,#2664,.F.);
#1462=ORIENTED_EDGE('',*,*,#2669,.T.);
#1463=ORIENTED_EDGE('',*,*,#2670,.F.);
#1464=ORIENTED_EDGE('',*,*,#2669,.F.);
#1465=ORIENTED_EDGE('',*,*,#2654,.T.);
#1466=ORIENTED_EDGE('',*,*,#2670,.T.);
#1467=ORIENTED_EDGE('',*,*,#2671,.T.);
#1468=ORIENTED_EDGE('',*,*,#2671,.F.);
#1469=ORIENTED_EDGE('',*,*,#2672,.T.);
#1470=ORIENTED_EDGE('',*,*,#2673,.F.);
#1471=ORIENTED_EDGE('',*,*,#2672,.F.);
#1472=ORIENTED_EDGE('',*,*,#2653,.T.);
#1473=ORIENTED_EDGE('',*,*,#2673,.T.);
#1474=ORIENTED_EDGE('',*,*,#2674,.T.);
#1475=ORIENTED_EDGE('',*,*,#2674,.F.);
#1476=ORIENTED_EDGE('',*,*,#2675,.F.);
#1477=ORIENTED_EDGE('',*,*,#2676,.F.);
#1478=ORIENTED_EDGE('',*,*,#2677,.T.);
#1479=ORIENTED_EDGE('',*,*,#2678,.T.);
#1480=ORIENTED_EDGE('',*,*,#2679,.T.);
#1481=ORIENTED_EDGE('',*,*,#2680,.F.);
#1482=ORIENTED_EDGE('',*,*,#2681,.F.);
#1483=ORIENTED_EDGE('',*,*,#2676,.T.);
#1484=ORIENTED_EDGE('',*,*,#2682,.T.);
#1485=ORIENTED_EDGE('',*,*,#2683,.F.);
#1486=ORIENTED_EDGE('',*,*,#2684,.F.);
#1487=ORIENTED_EDGE('',*,*,#2680,.T.);
#1488=ORIENTED_EDGE('',*,*,#2685,.F.);
#1489=ORIENTED_EDGE('',*,*,#2686,.T.);
#1490=ORIENTED_EDGE('',*,*,#2687,.F.);
#1491=ORIENTED_EDGE('',*,*,#2678,.F.);
#1492=ORIENTED_EDGE('',*,*,#2688,.T.);
#1493=ORIENTED_EDGE('',*,*,#2683,.T.);
#1494=ORIENTED_EDGE('',*,*,#2689,.F.);
#1495=ORIENTED_EDGE('',*,*,#2690,.T.);
#1496=ORIENTED_EDGE('',*,*,#2691,.F.);
#1497=ORIENTED_EDGE('',*,*,#2692,.T.);
#1498=ORIENTED_EDGE('',*,*,#2693,.T.);
#1499=ORIENTED_EDGE('',*,*,#2694,.F.);
#1500=ORIENTED_EDGE('',*,*,#2695,.T.);
#1501=ORIENTED_EDGE('',*,*,#2696,.F.);
#1502=ORIENTED_EDGE('',*,*,#2697,.T.);
#1503=ORIENTED_EDGE('',*,*,#2693,.F.);
#1504=ORIENTED_EDGE('',*,*,#2691,.T.);
#1505=ORIENTED_EDGE('',*,*,#2689,.T.);
#1506=ORIENTED_EDGE('',*,*,#2677,.F.);
#1507=ORIENTED_EDGE('',*,*,#2681,.T.);
#1508=ORIENTED_EDGE('',*,*,#2684,.T.);
#1509=ORIENTED_EDGE('',*,*,#2688,.F.);
#1510=ORIENTED_EDGE('',*,*,#2685,.T.);
#1511=ORIENTED_EDGE('',*,*,#2695,.F.);
#1512=ORIENTED_EDGE('',*,*,#2698,.F.);
#1513=ORIENTED_EDGE('',*,*,#2694,.T.);
#1514=ORIENTED_EDGE('',*,*,#2692,.F.);
#1515=ORIENTED_EDGE('',*,*,#2690,.F.);
#1516=ORIENTED_EDGE('',*,*,#2675,.T.);
#1517=ORIENTED_EDGE('',*,*,#2687,.T.);
#1518=ORIENTED_EDGE('',*,*,#2682,.F.);
#1519=ORIENTED_EDGE('',*,*,#2679,.F.);
#1520=ORIENTED_EDGE('',*,*,#2686,.F.);
#1521=ORIENTED_EDGE('',*,*,#2696,.T.);
#1522=ORIENTED_EDGE('',*,*,#2698,.T.);
#1523=ORIENTED_EDGE('',*,*,#2697,.F.);
#1524=ORIENTED_EDGE('',*,*,#2699,.F.);
#1525=ORIENTED_EDGE('',*,*,#2700,.F.);
#1526=ORIENTED_EDGE('',*,*,#2701,.F.);
#1527=ORIENTED_EDGE('',*,*,#2702,.T.);
#1528=ORIENTED_EDGE('',*,*,#2703,.T.);
#1529=ORIENTED_EDGE('',*,*,#2704,.T.);
#1530=ORIENTED_EDGE('',*,*,#2705,.T.);
#1531=ORIENTED_EDGE('',*,*,#2706,.F.);
#1532=ORIENTED_EDGE('',*,*,#2702,.F.);
#1533=ORIENTED_EDGE('',*,*,#2706,.T.);
#1534=ORIENTED_EDGE('',*,*,#2701,.T.);
#1535=ORIENTED_EDGE('',*,*,#2705,.F.);
#1536=ORIENTED_EDGE('',*,*,#2700,.T.);
#1537=ORIENTED_EDGE('',*,*,#2704,.F.);
#1538=ORIENTED_EDGE('',*,*,#2699,.T.);
#1539=ORIENTED_EDGE('',*,*,#2703,.F.);
#1540=ORIENTED_EDGE('',*,*,#2707,.T.);
#1541=ORIENTED_EDGE('',*,*,#2708,.T.);
#1542=ORIENTED_EDGE('',*,*,#2709,.T.);
#1543=ORIENTED_EDGE('',*,*,#2710,.F.);
#1544=ORIENTED_EDGE('',*,*,#2711,.F.);
#1545=ORIENTED_EDGE('',*,*,#2712,.F.);
#1546=ORIENTED_EDGE('',*,*,#2713,.F.);
#1547=ORIENTED_EDGE('',*,*,#2714,.F.);
#1548=ORIENTED_EDGE('',*,*,#2715,.F.);
#1549=ORIENTED_EDGE('',*,*,#2716,.F.);
#1550=ORIENTED_EDGE('',*,*,#2717,.F.);
#1551=ORIENTED_EDGE('',*,*,#2718,.F.);
#1552=ORIENTED_EDGE('',*,*,#2719,.F.);
#1553=ORIENTED_EDGE('',*,*,#2720,.F.);
#1554=ORIENTED_EDGE('',*,*,#2721,.F.);
#1555=ORIENTED_EDGE('',*,*,#2722,.F.);
#1556=ORIENTED_EDGE('',*,*,#2723,.F.);
#1557=ORIENTED_EDGE('',*,*,#2724,.F.);
#1558=ORIENTED_EDGE('',*,*,#2725,.F.);
#1559=ORIENTED_EDGE('',*,*,#2726,.F.);
#1560=ORIENTED_EDGE('',*,*,#2727,.F.);
#1561=ORIENTED_EDGE('',*,*,#2728,.F.);
#1562=ORIENTED_EDGE('',*,*,#2729,.F.);
#1563=ORIENTED_EDGE('',*,*,#2730,.F.);
#1564=ORIENTED_EDGE('',*,*,#2731,.F.);
#1565=ORIENTED_EDGE('',*,*,#2732,.F.);
#1566=ORIENTED_EDGE('',*,*,#2733,.F.);
#1567=ORIENTED_EDGE('',*,*,#2734,.F.);
#1568=ORIENTED_EDGE('',*,*,#2735,.F.);
#1569=ORIENTED_EDGE('',*,*,#2736,.F.);
#1570=ORIENTED_EDGE('',*,*,#2737,.F.);
#1571=ORIENTED_EDGE('',*,*,#2738,.F.);
#1572=ORIENTED_EDGE('',*,*,#2739,.F.);
#1573=ORIENTED_EDGE('',*,*,#2740,.F.);
#1574=ORIENTED_EDGE('',*,*,#2741,.F.);
#1575=ORIENTED_EDGE('',*,*,#2742,.F.);
#1576=ORIENTED_EDGE('',*,*,#2743,.F.);
#1577=ORIENTED_EDGE('',*,*,#2744,.F.);
#1578=ORIENTED_EDGE('',*,*,#2745,.F.);
#1579=ORIENTED_EDGE('',*,*,#2746,.F.);
#1580=ORIENTED_EDGE('',*,*,#2747,.F.);
#1581=ORIENTED_EDGE('',*,*,#2748,.F.);
#1582=ORIENTED_EDGE('',*,*,#2749,.F.);
#1583=ORIENTED_EDGE('',*,*,#2750,.F.);
#1584=ORIENTED_EDGE('',*,*,#2751,.F.);
#1585=ORIENTED_EDGE('',*,*,#2752,.F.);
#1586=ORIENTED_EDGE('',*,*,#2753,.F.);
#1587=ORIENTED_EDGE('',*,*,#2754,.F.);
#1588=ORIENTED_EDGE('',*,*,#2755,.F.);
#1589=ORIENTED_EDGE('',*,*,#2756,.F.);
#1590=ORIENTED_EDGE('',*,*,#2757,.F.);
#1591=ORIENTED_EDGE('',*,*,#2758,.F.);
#1592=ORIENTED_EDGE('',*,*,#2759,.F.);
#1593=ORIENTED_EDGE('',*,*,#2760,.F.);
#1594=ORIENTED_EDGE('',*,*,#2761,.F.);
#1595=ORIENTED_EDGE('',*,*,#2762,.F.);
#1596=ORIENTED_EDGE('',*,*,#2763,.F.);
#1597=ORIENTED_EDGE('',*,*,#2764,.F.);
#1598=ORIENTED_EDGE('',*,*,#2765,.F.);
#1599=ORIENTED_EDGE('',*,*,#2766,.F.);
#1600=ORIENTED_EDGE('',*,*,#2767,.F.);
#1601=ORIENTED_EDGE('',*,*,#2768,.F.);
#1602=ORIENTED_EDGE('',*,*,#2769,.F.);
#1603=ORIENTED_EDGE('',*,*,#2770,.F.);
#1604=ORIENTED_EDGE('',*,*,#2771,.F.);
#1605=ORIENTED_EDGE('',*,*,#2772,.F.);
#1606=ORIENTED_EDGE('',*,*,#2773,.F.);
#1607=ORIENTED_EDGE('',*,*,#2774,.F.);
#1608=ORIENTED_EDGE('',*,*,#2775,.F.);
#1609=ORIENTED_EDGE('',*,*,#2776,.F.);
#1610=ORIENTED_EDGE('',*,*,#2777,.F.);
#1611=ORIENTED_EDGE('',*,*,#2778,.F.);
#1612=ORIENTED_EDGE('',*,*,#2779,.F.);
#1613=ORIENTED_EDGE('',*,*,#2780,.F.);
#1614=ORIENTED_EDGE('',*,*,#2781,.F.);
#1615=ORIENTED_EDGE('',*,*,#2782,.F.);
#1616=ORIENTED_EDGE('',*,*,#2783,.F.);
#1617=ORIENTED_EDGE('',*,*,#2784,.F.);
#1618=ORIENTED_EDGE('',*,*,#2785,.F.);
#1619=ORIENTED_EDGE('',*,*,#2786,.F.);
#1620=ORIENTED_EDGE('',*,*,#2787,.F.);
#1621=ORIENTED_EDGE('',*,*,#2788,.F.);
#1622=ORIENTED_EDGE('',*,*,#2789,.F.);
#1623=ORIENTED_EDGE('',*,*,#2790,.F.);
#1624=ORIENTED_EDGE('',*,*,#2791,.F.);
#1625=ORIENTED_EDGE('',*,*,#2792,.F.);
#1626=ORIENTED_EDGE('',*,*,#2793,.F.);
#1627=ORIENTED_EDGE('',*,*,#2794,.F.);
#1628=ORIENTED_EDGE('',*,*,#2795,.F.);
#1629=ORIENTED_EDGE('',*,*,#2796,.F.);
#1630=ORIENTED_EDGE('',*,*,#2797,.F.);
#1631=ORIENTED_EDGE('',*,*,#2798,.F.);
#1632=ORIENTED_EDGE('',*,*,#2709,.F.);
#1633=ORIENTED_EDGE('',*,*,#2799,.F.);
#1634=ORIENTED_EDGE('',*,*,#2798,.T.);
#1635=ORIENTED_EDGE('',*,*,#2800,.F.);
#1636=ORIENTED_EDGE('',*,*,#2801,.F.);
#1637=ORIENTED_EDGE('',*,*,#2802,.F.);
#1638=ORIENTED_EDGE('',*,*,#2803,.F.);
#1639=ORIENTED_EDGE('',*,*,#2804,.F.);
#1640=ORIENTED_EDGE('',*,*,#2714,.T.);
#1641=ORIENTED_EDGE('',*,*,#2805,.F.);
#1642=ORIENTED_EDGE('',*,*,#2794,.T.);
#1643=ORIENTED_EDGE('',*,*,#2806,.F.);
#1644=ORIENTED_EDGE('',*,*,#2807,.F.);
#1645=ORIENTED_EDGE('',*,*,#2808,.F.);
#1646=ORIENTED_EDGE('',*,*,#2790,.T.);
#1647=ORIENTED_EDGE('',*,*,#2809,.F.);
#1648=ORIENTED_EDGE('',*,*,#2810,.F.);
#1649=ORIENTED_EDGE('',*,*,#2811,.F.);
#1650=ORIENTED_EDGE('',*,*,#2782,.T.);
#1651=ORIENTED_EDGE('',*,*,#2812,.F.);
#1652=ORIENTED_EDGE('',*,*,#2813,.F.);
#1653=ORIENTED_EDGE('',*,*,#2814,.F.);
#1654=ORIENTED_EDGE('',*,*,#2815,.F.);
#1655=ORIENTED_EDGE('',*,*,#2816,.F.);
#1656=ORIENTED_EDGE('',*,*,#2786,.T.);
#1657=ORIENTED_EDGE('',*,*,#2817,.F.);
#1658=ORIENTED_EDGE('',*,*,#2730,.T.);
#1659=ORIENTED_EDGE('',*,*,#2818,.F.);
#1660=ORIENTED_EDGE('',*,*,#2819,.F.);
#1661=ORIENTED_EDGE('',*,*,#2820,.F.);
#1662=ORIENTED_EDGE('',*,*,#2821,.F.);
#1663=ORIENTED_EDGE('',*,*,#2822,.F.);
#1664=ORIENTED_EDGE('',*,*,#2734,.T.);
#1665=ORIENTED_EDGE('',*,*,#2823,.F.);
#1666=ORIENTED_EDGE('',*,*,#2726,.T.);
#1667=ORIENTED_EDGE('',*,*,#2824,.F.);
#1668=ORIENTED_EDGE('',*,*,#2825,.F.);
#1669=ORIENTED_EDGE('',*,*,#2826,.F.);
#1670=ORIENTED_EDGE('',*,*,#2722,.T.);
#1671=ORIENTED_EDGE('',*,*,#2827,.F.);
#1672=ORIENTED_EDGE('',*,*,#2828,.F.);
#1673=ORIENTED_EDGE('',*,*,#2829,.F.);
#1674=ORIENTED_EDGE('',*,*,#2830,.F.);
#1675=ORIENTED_EDGE('',*,*,#2831,.F.);
#1676=ORIENTED_EDGE('',*,*,#2718,.T.);
#1677=ORIENTED_EDGE('',*,*,#2832,.F.);
#1678=ORIENTED_EDGE('',*,*,#2742,.T.);
#1679=ORIENTED_EDGE('',*,*,#2833,.F.);
#1680=ORIENTED_EDGE('',*,*,#2834,.F.);
#1681=ORIENTED_EDGE('',*,*,#2835,.F.);
#1682=ORIENTED_EDGE('',*,*,#2836,.F.);
#1683=ORIENTED_EDGE('',*,*,#2837,.F.);
#1684=ORIENTED_EDGE('',*,*,#2746,.T.);
#1685=ORIENTED_EDGE('',*,*,#2838,.F.);
#1686=ORIENTED_EDGE('',*,*,#2839,.F.);
#1687=ORIENTED_EDGE('',*,*,#2840,.F.);
#1688=ORIENTED_EDGE('',*,*,#2750,.T.);
#1689=ORIENTED_EDGE('',*,*,#2841,.F.);
#1690=ORIENTED_EDGE('',*,*,#2842,.F.);
#1691=ORIENTED_EDGE('',*,*,#2843,.F.);
#1692=ORIENTED_EDGE('',*,*,#2754,.T.);
#1693=ORIENTED_EDGE('',*,*,#2844,.F.);
#1694=ORIENTED_EDGE('',*,*,#2738,.T.);
#1695=ORIENTED_EDGE('',*,*,#2845,.F.);
#1696=ORIENTED_EDGE('',*,*,#2846,.F.);
#1697=ORIENTED_EDGE('',*,*,#2847,.F.);
#1698=ORIENTED_EDGE('',*,*,#2762,.T.);
#1699=ORIENTED_EDGE('',*,*,#2848,.F.);
#1700=ORIENTED_EDGE('',*,*,#2849,.F.);
#1701=ORIENTED_EDGE('',*,*,#2850,.F.);
#1702=ORIENTED_EDGE('',*,*,#2851,.F.);
#1703=ORIENTED_EDGE('',*,*,#2852,.F.);
#1704=ORIENTED_EDGE('',*,*,#2766,.T.);
#1705=ORIENTED_EDGE('',*,*,#2853,.F.);
#1706=ORIENTED_EDGE('',*,*,#2854,.F.);
#1707=ORIENTED_EDGE('',*,*,#2855,.F.);
#1708=ORIENTED_EDGE('',*,*,#2770,.T.);
#1709=ORIENTED_EDGE('',*,*,#2856,.F.);
#1710=ORIENTED_EDGE('',*,*,#2857,.F.);
#1711=ORIENTED_EDGE('',*,*,#2858,.F.);
#1712=ORIENTED_EDGE('',*,*,#2774,.T.);
#1713=ORIENTED_EDGE('',*,*,#2859,.F.);
#1714=ORIENTED_EDGE('',*,*,#2758,.T.);
#1715=ORIENTED_EDGE('',*,*,#2860,.F.);
#1716=ORIENTED_EDGE('',*,*,#2861,.F.);
#1717=ORIENTED_EDGE('',*,*,#2707,.F.);
#1718=ORIENTED_EDGE('',*,*,#2862,.T.);
#1719=ORIENTED_EDGE('',*,*,#2801,.T.);
#1720=ORIENTED_EDGE('',*,*,#2863,.F.);
#1721=ORIENTED_EDGE('',*,*,#2864,.T.);
#1722=ORIENTED_EDGE('',*,*,#2865,.T.);
#1723=ORIENTED_EDGE('',*,*,#2807,.T.);
#1724=ORIENTED_EDGE('',*,*,#2866,.F.);
#1725=ORIENTED_EDGE('',*,*,#2867,.T.);
#1726=ORIENTED_EDGE('',*,*,#2868,.T.);
#1727=ORIENTED_EDGE('',*,*,#2810,.T.);
#1728=ORIENTED_EDGE('',*,*,#2869,.F.);
#1729=ORIENTED_EDGE('',*,*,#2870,.T.);
#1730=ORIENTED_EDGE('',*,*,#2871,.T.);
#1731=ORIENTED_EDGE('',*,*,#2815,.T.);
#1732=ORIENTED_EDGE('',*,*,#2872,.F.);
#1733=ORIENTED_EDGE('',*,*,#2873,.T.);
#1734=ORIENTED_EDGE('',*,*,#2874,.T.);
#1735=ORIENTED_EDGE('',*,*,#2813,.T.);
#1736=ORIENTED_EDGE('',*,*,#2875,.F.);
#1737=ORIENTED_EDGE('',*,*,#2876,.T.);
#1738=ORIENTED_EDGE('',*,*,#2877,.T.);
#1739=ORIENTED_EDGE('',*,*,#2878,.T.);
#1740=ORIENTED_EDGE('',*,*,#2879,.F.);
#1741=ORIENTED_EDGE('',*,*,#2880,.T.);
#1742=ORIENTED_EDGE('',*,*,#2881,.T.);
#1743=ORIENTED_EDGE('',*,*,#2857,.T.);
#1744=ORIENTED_EDGE('',*,*,#2882,.F.);
#1745=ORIENTED_EDGE('',*,*,#2883,.T.);
#1746=ORIENTED_EDGE('',*,*,#2884,.T.);
#1747=ORIENTED_EDGE('',*,*,#2854,.T.);
#1748=ORIENTED_EDGE('',*,*,#2885,.F.);
#1749=ORIENTED_EDGE('',*,*,#2886,.T.);
#1750=ORIENTED_EDGE('',*,*,#2887,.T.);
#1751=ORIENTED_EDGE('',*,*,#2851,.T.);
#1752=ORIENTED_EDGE('',*,*,#2888,.F.);
#1753=ORIENTED_EDGE('',*,*,#2889,.T.);
#1754=ORIENTED_EDGE('',*,*,#2890,.T.);
#1755=ORIENTED_EDGE('',*,*,#2849,.T.);
#1756=ORIENTED_EDGE('',*,*,#2891,.F.);
#1757=ORIENTED_EDGE('',*,*,#2892,.T.);
#1758=ORIENTED_EDGE('',*,*,#2893,.T.);
#1759=ORIENTED_EDGE('',*,*,#2861,.T.);
#1760=ORIENTED_EDGE('',*,*,#2894,.F.);
#1761=ORIENTED_EDGE('',*,*,#2895,.T.);
#1762=ORIENTED_EDGE('',*,*,#2896,.T.);
#1763=ORIENTED_EDGE('',*,*,#2842,.T.);
#1764=ORIENTED_EDGE('',*,*,#2897,.F.);
#1765=ORIENTED_EDGE('',*,*,#2898,.T.);
#1766=ORIENTED_EDGE('',*,*,#2899,.T.);
#1767=ORIENTED_EDGE('',*,*,#2839,.T.);
#1768=ORIENTED_EDGE('',*,*,#2900,.F.);
#1769=ORIENTED_EDGE('',*,*,#2901,.T.);
#1770=ORIENTED_EDGE('',*,*,#2902,.T.);
#1771=ORIENTED_EDGE('',*,*,#2836,.T.);
#1772=ORIENTED_EDGE('',*,*,#2903,.F.);
#1773=ORIENTED_EDGE('',*,*,#2904,.T.);
#1774=ORIENTED_EDGE('',*,*,#2905,.T.);
#1775=ORIENTED_EDGE('',*,*,#2834,.T.);
#1776=ORIENTED_EDGE('',*,*,#2906,.F.);
#1777=ORIENTED_EDGE('',*,*,#2907,.T.);
#1778=ORIENTED_EDGE('',*,*,#2908,.T.);
#1779=ORIENTED_EDGE('',*,*,#2846,.T.);
#1780=ORIENTED_EDGE('',*,*,#2909,.F.);
#1781=ORIENTED_EDGE('',*,*,#2910,.T.);
#1782=ORIENTED_EDGE('',*,*,#2911,.T.);
#1783=ORIENTED_EDGE('',*,*,#2821,.T.);
#1784=ORIENTED_EDGE('',*,*,#2912,.F.);
#1785=ORIENTED_EDGE('',*,*,#2913,.T.);
#1786=ORIENTED_EDGE('',*,*,#2914,.T.);
#1787=ORIENTED_EDGE('',*,*,#2819,.T.);
#1788=ORIENTED_EDGE('',*,*,#2915,.F.);
#1789=ORIENTED_EDGE('',*,*,#2916,.T.);
#1790=ORIENTED_EDGE('',*,*,#2917,.T.);
#1791=ORIENTED_EDGE('',*,*,#2825,.T.);
#1792=ORIENTED_EDGE('',*,*,#2918,.F.);
#1793=ORIENTED_EDGE('',*,*,#2919,.T.);
#1794=ORIENTED_EDGE('',*,*,#2920,.T.);
#1795=ORIENTED_EDGE('',*,*,#2828,.T.);
#1796=ORIENTED_EDGE('',*,*,#2921,.F.);
#1797=ORIENTED_EDGE('',*,*,#2922,.T.);
#1798=ORIENTED_EDGE('',*,*,#2923,.T.);
#1799=ORIENTED_EDGE('',*,*,#2830,.T.);
#1800=ORIENTED_EDGE('',*,*,#2924,.F.);
#1801=ORIENTED_EDGE('',*,*,#2925,.T.);
#1802=ORIENTED_EDGE('',*,*,#2926,.T.);
#1803=ORIENTED_EDGE('',*,*,#2803,.T.);
#1804=ORIENTED_EDGE('',*,*,#2927,.F.);
#1805=ORIENTED_EDGE('',*,*,#2928,.T.);
#1806=ORIENTED_EDGE('',*,*,#2929,.F.);
#1807=ORIENTED_EDGE('',*,*,#2778,.T.);
#1808=ORIENTED_EDGE('',*,*,#2930,.F.);
#1809=ORIENTED_EDGE('',*,*,#2878,.F.);
#1810=ORIENTED_EDGE('',*,*,#2858,.T.);
#1811=ORIENTED_EDGE('',*,*,#2881,.F.);
#1812=ORIENTED_EDGE('',*,*,#2931,.F.);
#1813=ORIENTED_EDGE('',*,*,#2775,.T.);
#1814=ORIENTED_EDGE('',*,*,#2930,.T.);
#1815=ORIENTED_EDGE('',*,*,#2777,.T.);
#1816=ORIENTED_EDGE('',*,*,#2932,.T.);
#1817=ORIENTED_EDGE('',*,*,#2879,.T.);
#1818=ORIENTED_EDGE('',*,*,#2880,.F.);
#1819=ORIENTED_EDGE('',*,*,#2932,.F.);
#1820=ORIENTED_EDGE('',*,*,#2776,.T.);
#1821=ORIENTED_EDGE('',*,*,#2931,.T.);
#1822=ORIENTED_EDGE('',*,*,#2929,.T.);
#1823=ORIENTED_EDGE('',*,*,#2877,.F.);
#1824=ORIENTED_EDGE('',*,*,#2933,.F.);
#1825=ORIENTED_EDGE('',*,*,#2779,.T.);
#1826=ORIENTED_EDGE('',*,*,#2812,.T.);
#1827=ORIENTED_EDGE('',*,*,#2781,.T.);
#1828=ORIENTED_EDGE('',*,*,#2934,.T.);
#1829=ORIENTED_EDGE('',*,*,#2875,.T.);
#1830=ORIENTED_EDGE('',*,*,#2876,.F.);
#1831=ORIENTED_EDGE('',*,*,#2934,.F.);
#1832=ORIENTED_EDGE('',*,*,#2780,.T.);
#1833=ORIENTED_EDGE('',*,*,#2933,.T.);
#1834=ORIENTED_EDGE('',*,*,#2843,.T.);
#1835=ORIENTED_EDGE('',*,*,#2896,.F.);
#1836=ORIENTED_EDGE('',*,*,#2935,.F.);
#1837=ORIENTED_EDGE('',*,*,#2755,.T.);
#1838=ORIENTED_EDGE('',*,*,#2860,.T.);
#1839=ORIENTED_EDGE('',*,*,#2757,.T.);
#1840=ORIENTED_EDGE('',*,*,#2936,.T.);
#1841=ORIENTED_EDGE('',*,*,#2894,.T.);
#1842=ORIENTED_EDGE('',*,*,#2895,.F.);
#1843=ORIENTED_EDGE('',*,*,#2936,.F.);
#1844=ORIENTED_EDGE('',*,*,#2756,.T.);
#1845=ORIENTED_EDGE('',*,*,#2935,.T.);
#1846=ORIENTED_EDGE('',*,*,#2859,.T.);
#1847=ORIENTED_EDGE('',*,*,#2893,.F.);
#1848=ORIENTED_EDGE('',*,*,#2937,.F.);
#1849=ORIENTED_EDGE('',*,*,#2759,.T.);
#1850=ORIENTED_EDGE('',*,*,#2848,.T.);
#1851=ORIENTED_EDGE('',*,*,#2761,.T.);
#1852=ORIENTED_EDGE('',*,*,#2938,.T.);
#1853=ORIENTED_EDGE('',*,*,#2891,.T.);
#1854=ORIENTED_EDGE('',*,*,#2892,.F.);
#1855=ORIENTED_EDGE('',*,*,#2938,.F.);
#1856=ORIENTED_EDGE('',*,*,#2760,.T.);
#1857=ORIENTED_EDGE('',*,*,#2937,.T.);
#1858=ORIENTED_EDGE('',*,*,#2855,.T.);
#1859=ORIENTED_EDGE('',*,*,#2884,.F.);
#1860=ORIENTED_EDGE('',*,*,#2939,.F.);
#1861=ORIENTED_EDGE('',*,*,#2771,.T.);
#1862=ORIENTED_EDGE('',*,*,#2856,.T.);
#1863=ORIENTED_EDGE('',*,*,#2773,.T.);
#1864=ORIENTED_EDGE('',*,*,#2940,.T.);
#1865=ORIENTED_EDGE('',*,*,#2882,.T.);
#1866=ORIENTED_EDGE('',*,*,#2883,.F.);
#1867=ORIENTED_EDGE('',*,*,#2940,.F.);
#1868=ORIENTED_EDGE('',*,*,#2772,.T.);
#1869=ORIENTED_EDGE('',*,*,#2939,.T.);
#1870=ORIENTED_EDGE('',*,*,#2852,.T.);
#1871=ORIENTED_EDGE('',*,*,#2887,.F.);
#1872=ORIENTED_EDGE('',*,*,#2941,.F.);
#1873=ORIENTED_EDGE('',*,*,#2767,.T.);
#1874=ORIENTED_EDGE('',*,*,#2853,.T.);
#1875=ORIENTED_EDGE('',*,*,#2769,.T.);
#1876=ORIENTED_EDGE('',*,*,#2942,.T.);
#1877=ORIENTED_EDGE('',*,*,#2885,.T.);
#1878=ORIENTED_EDGE('',*,*,#2886,.F.);
#1879=ORIENTED_EDGE('',*,*,#2942,.F.);
#1880=ORIENTED_EDGE('',*,*,#2768,.T.);
#1881=ORIENTED_EDGE('',*,*,#2941,.T.);
#1882=ORIENTED_EDGE('',*,*,#2847,.T.);
#1883=ORIENTED_EDGE('',*,*,#2890,.F.);
#1884=ORIENTED_EDGE('',*,*,#2943,.F.);
#1885=ORIENTED_EDGE('',*,*,#2763,.T.);
#1886=ORIENTED_EDGE('',*,*,#2850,.T.);
#1887=ORIENTED_EDGE('',*,*,#2765,.T.);
#1888=ORIENTED_EDGE('',*,*,#2944,.T.);
#1889=ORIENTED_EDGE('',*,*,#2888,.T.);
#1890=ORIENTED_EDGE('',*,*,#2889,.F.);
#1891=ORIENTED_EDGE('',*,*,#2944,.F.);
#1892=ORIENTED_EDGE('',*,*,#2764,.T.);
#1893=ORIENTED_EDGE('',*,*,#2943,.T.);
#1894=ORIENTED_EDGE('',*,*,#2822,.T.);
#1895=ORIENTED_EDGE('',*,*,#2911,.F.);
#1896=ORIENTED_EDGE('',*,*,#2945,.F.);
#1897=ORIENTED_EDGE('',*,*,#2735,.T.);
#1898=ORIENTED_EDGE('',*,*,#2845,.T.);
#1899=ORIENTED_EDGE('',*,*,#2737,.T.);
#1900=ORIENTED_EDGE('',*,*,#2946,.T.);
#1901=ORIENTED_EDGE('',*,*,#2909,.T.);
#1902=ORIENTED_EDGE('',*,*,#2910,.F.);
#1903=ORIENTED_EDGE('',*,*,#2946,.F.);
#1904=ORIENTED_EDGE('',*,*,#2736,.T.);
#1905=ORIENTED_EDGE('',*,*,#2945,.T.);
#1906=ORIENTED_EDGE('',*,*,#2844,.T.);
#1907=ORIENTED_EDGE('',*,*,#2908,.F.);
#1908=ORIENTED_EDGE('',*,*,#2947,.F.);
#1909=ORIENTED_EDGE('',*,*,#2739,.T.);
#1910=ORIENTED_EDGE('',*,*,#2833,.T.);
#1911=ORIENTED_EDGE('',*,*,#2741,.T.);
#1912=ORIENTED_EDGE('',*,*,#2948,.T.);
#1913=ORIENTED_EDGE('',*,*,#2906,.T.);
#1914=ORIENTED_EDGE('',*,*,#2907,.F.);
#1915=ORIENTED_EDGE('',*,*,#2948,.F.);
#1916=ORIENTED_EDGE('',*,*,#2740,.T.);
#1917=ORIENTED_EDGE('',*,*,#2947,.T.);
#1918=ORIENTED_EDGE('',*,*,#2840,.T.);
#1919=ORIENTED_EDGE('',*,*,#2899,.F.);
#1920=ORIENTED_EDGE('',*,*,#2949,.F.);
#1921=ORIENTED_EDGE('',*,*,#2751,.T.);
#1922=ORIENTED_EDGE('',*,*,#2841,.T.);
#1923=ORIENTED_EDGE('',*,*,#2753,.T.);
#1924=ORIENTED_EDGE('',*,*,#2950,.T.);
#1925=ORIENTED_EDGE('',*,*,#2897,.T.);
#1926=ORIENTED_EDGE('',*,*,#2898,.F.);
#1927=ORIENTED_EDGE('',*,*,#2950,.F.);
#1928=ORIENTED_EDGE('',*,*,#2752,.T.);
#1929=ORIENTED_EDGE('',*,*,#2949,.T.);
#1930=ORIENTED_EDGE('',*,*,#2837,.T.);
#1931=ORIENTED_EDGE('',*,*,#2902,.F.);
#1932=ORIENTED_EDGE('',*,*,#2951,.F.);
#1933=ORIENTED_EDGE('',*,*,#2747,.T.);
#1934=ORIENTED_EDGE('',*,*,#2838,.T.);
#1935=ORIENTED_EDGE('',*,*,#2749,.T.);
#1936=ORIENTED_EDGE('',*,*,#2952,.T.);
#1937=ORIENTED_EDGE('',*,*,#2900,.T.);
#1938=ORIENTED_EDGE('',*,*,#2901,.F.);
#1939=ORIENTED_EDGE('',*,*,#2952,.F.);
#1940=ORIENTED_EDGE('',*,*,#2748,.T.);
#1941=ORIENTED_EDGE('',*,*,#2951,.T.);
#1942=ORIENTED_EDGE('',*,*,#2832,.T.);
#1943=ORIENTED_EDGE('',*,*,#2905,.F.);
#1944=ORIENTED_EDGE('',*,*,#2953,.F.);
#1945=ORIENTED_EDGE('',*,*,#2743,.T.);
#1946=ORIENTED_EDGE('',*,*,#2835,.T.);
#1947=ORIENTED_EDGE('',*,*,#2745,.T.);
#1948=ORIENTED_EDGE('',*,*,#2954,.T.);
#1949=ORIENTED_EDGE('',*,*,#2903,.T.);
#1950=ORIENTED_EDGE('',*,*,#2904,.F.);
#1951=ORIENTED_EDGE('',*,*,#2954,.F.);
#1952=ORIENTED_EDGE('',*,*,#2744,.T.);
#1953=ORIENTED_EDGE('',*,*,#2953,.T.);
#1954=ORIENTED_EDGE('',*,*,#2831,.T.);
#1955=ORIENTED_EDGE('',*,*,#2923,.F.);
#1956=ORIENTED_EDGE('',*,*,#2955,.F.);
#1957=ORIENTED_EDGE('',*,*,#2719,.T.);
#1958=ORIENTED_EDGE('',*,*,#2827,.T.);
#1959=ORIENTED_EDGE('',*,*,#2721,.T.);
#1960=ORIENTED_EDGE('',*,*,#2956,.T.);
#1961=ORIENTED_EDGE('',*,*,#2921,.T.);
#1962=ORIENTED_EDGE('',*,*,#2922,.F.);
#1963=ORIENTED_EDGE('',*,*,#2956,.F.);
#1964=ORIENTED_EDGE('',*,*,#2720,.T.);
#1965=ORIENTED_EDGE('',*,*,#2955,.T.);
#1966=ORIENTED_EDGE('',*,*,#2804,.T.);
#1967=ORIENTED_EDGE('',*,*,#2926,.F.);
#1968=ORIENTED_EDGE('',*,*,#2957,.F.);
#1969=ORIENTED_EDGE('',*,*,#2715,.T.);
#1970=ORIENTED_EDGE('',*,*,#2829,.T.);
#1971=ORIENTED_EDGE('',*,*,#2717,.T.);
#1972=ORIENTED_EDGE('',*,*,#2958,.T.);
#1973=ORIENTED_EDGE('',*,*,#2924,.T.);
#1974=ORIENTED_EDGE('',*,*,#2925,.F.);
#1975=ORIENTED_EDGE('',*,*,#2958,.F.);
#1976=ORIENTED_EDGE('',*,*,#2716,.T.);
#1977=ORIENTED_EDGE('',*,*,#2957,.T.);
#1978=ORIENTED_EDGE('',*,*,#2826,.T.);
#1979=ORIENTED_EDGE('',*,*,#2920,.F.);
#1980=ORIENTED_EDGE('',*,*,#2959,.F.);
#1981=ORIENTED_EDGE('',*,*,#2723,.T.);
#1982=ORIENTED_EDGE('',*,*,#2824,.T.);
#1983=ORIENTED_EDGE('',*,*,#2725,.T.);
#1984=ORIENTED_EDGE('',*,*,#2960,.T.);
#1985=ORIENTED_EDGE('',*,*,#2918,.T.);
#1986=ORIENTED_EDGE('',*,*,#2919,.F.);
#1987=ORIENTED_EDGE('',*,*,#2960,.F.);
#1988=ORIENTED_EDGE('',*,*,#2724,.T.);
#1989=ORIENTED_EDGE('',*,*,#2959,.T.);
#1990=ORIENTED_EDGE('',*,*,#2823,.T.);
#1991=ORIENTED_EDGE('',*,*,#2917,.F.);
#1992=ORIENTED_EDGE('',*,*,#2961,.F.);
#1993=ORIENTED_EDGE('',*,*,#2727,.T.);
#1994=ORIENTED_EDGE('',*,*,#2818,.T.);
#1995=ORIENTED_EDGE('',*,*,#2729,.T.);
#1996=ORIENTED_EDGE('',*,*,#2962,.T.);
#1997=ORIENTED_EDGE('',*,*,#2915,.T.);
#1998=ORIENTED_EDGE('',*,*,#2916,.F.);
#1999=ORIENTED_EDGE('',*,*,#2962,.F.);
#2000=ORIENTED_EDGE('',*,*,#2728,.T.);
#2001=ORIENTED_EDGE('',*,*,#2961,.T.);
#2002=ORIENTED_EDGE('',*,*,#2817,.T.);
#2003=ORIENTED_EDGE('',*,*,#2914,.F.);
#2004=ORIENTED_EDGE('',*,*,#2963,.F.);
#2005=ORIENTED_EDGE('',*,*,#2731,.T.);
#2006=ORIENTED_EDGE('',*,*,#2820,.T.);
#2007=ORIENTED_EDGE('',*,*,#2733,.T.);
#2008=ORIENTED_EDGE('',*,*,#2964,.T.);
#2009=ORIENTED_EDGE('',*,*,#2912,.T.);
#2010=ORIENTED_EDGE('',*,*,#2913,.F.);
#2011=ORIENTED_EDGE('',*,*,#2964,.F.);
#2012=ORIENTED_EDGE('',*,*,#2732,.T.);
#2013=ORIENTED_EDGE('',*,*,#2963,.T.);
#2014=ORIENTED_EDGE('',*,*,#2816,.T.);
#2015=ORIENTED_EDGE('',*,*,#2871,.F.);
#2016=ORIENTED_EDGE('',*,*,#2965,.F.);
#2017=ORIENTED_EDGE('',*,*,#2787,.T.);
#2018=ORIENTED_EDGE('',*,*,#2809,.T.);
#2019=ORIENTED_EDGE('',*,*,#2789,.T.);
#2020=ORIENTED_EDGE('',*,*,#2966,.T.);
#2021=ORIENTED_EDGE('',*,*,#2869,.T.);
#2022=ORIENTED_EDGE('',*,*,#2870,.F.);
#2023=ORIENTED_EDGE('',*,*,#2966,.F.);
#2024=ORIENTED_EDGE('',*,*,#2788,.T.);
#2025=ORIENTED_EDGE('',*,*,#2965,.T.);
#2026=ORIENTED_EDGE('',*,*,#2811,.T.);
#2027=ORIENTED_EDGE('',*,*,#2874,.F.);
#2028=ORIENTED_EDGE('',*,*,#2967,.F.);
#2029=ORIENTED_EDGE('',*,*,#2783,.T.);
#2030=ORIENTED_EDGE('',*,*,#2814,.T.);
#2031=ORIENTED_EDGE('',*,*,#2785,.T.);
#2032=ORIENTED_EDGE('',*,*,#2968,.T.);
#2033=ORIENTED_EDGE('',*,*,#2872,.T.);
#2034=ORIENTED_EDGE('',*,*,#2873,.F.);
#2035=ORIENTED_EDGE('',*,*,#2968,.F.);
#2036=ORIENTED_EDGE('',*,*,#2784,.T.);
#2037=ORIENTED_EDGE('',*,*,#2967,.T.);
#2038=ORIENTED_EDGE('',*,*,#2808,.T.);
#2039=ORIENTED_EDGE('',*,*,#2868,.F.);
#2040=ORIENTED_EDGE('',*,*,#2969,.F.);
#2041=ORIENTED_EDGE('',*,*,#2791,.T.);
#2042=ORIENTED_EDGE('',*,*,#2806,.T.);
#2043=ORIENTED_EDGE('',*,*,#2793,.T.);
#2044=ORIENTED_EDGE('',*,*,#2970,.T.);
#2045=ORIENTED_EDGE('',*,*,#2866,.T.);
#2046=ORIENTED_EDGE('',*,*,#2867,.F.);
#2047=ORIENTED_EDGE('',*,*,#2970,.F.);
#2048=ORIENTED_EDGE('',*,*,#2792,.T.);
#2049=ORIENTED_EDGE('',*,*,#2969,.T.);
#2050=ORIENTED_EDGE('',*,*,#2805,.T.);
#2051=ORIENTED_EDGE('',*,*,#2865,.F.);
#2052=ORIENTED_EDGE('',*,*,#2971,.F.);
#2053=ORIENTED_EDGE('',*,*,#2795,.T.);
#2054=ORIENTED_EDGE('',*,*,#2800,.T.);
#2055=ORIENTED_EDGE('',*,*,#2797,.T.);
#2056=ORIENTED_EDGE('',*,*,#2972,.T.);
#2057=ORIENTED_EDGE('',*,*,#2863,.T.);
#2058=ORIENTED_EDGE('',*,*,#2864,.F.);
#2059=ORIENTED_EDGE('',*,*,#2972,.F.);
#2060=ORIENTED_EDGE('',*,*,#2796,.T.);
#2061=ORIENTED_EDGE('',*,*,#2971,.T.);
#2062=ORIENTED_EDGE('',*,*,#2799,.T.);
#2063=ORIENTED_EDGE('',*,*,#2862,.F.);
#2064=ORIENTED_EDGE('',*,*,#2973,.F.);
#2065=ORIENTED_EDGE('',*,*,#2711,.T.);
#2066=ORIENTED_EDGE('',*,*,#2802,.T.);
#2067=ORIENTED_EDGE('',*,*,#2713,.T.);
#2068=ORIENTED_EDGE('',*,*,#2974,.T.);
#2069=ORIENTED_EDGE('',*,*,#2927,.T.);
#2070=ORIENTED_EDGE('',*,*,#2928,.F.);
#2071=ORIENTED_EDGE('',*,*,#2974,.F.);
#2072=ORIENTED_EDGE('',*,*,#2712,.T.);
#2073=ORIENTED_EDGE('',*,*,#2973,.T.);
#2074=ORIENTED_EDGE('',*,*,#2975,.F.);
#2075=ORIENTED_EDGE('',*,*,#2976,.T.);
#2076=ORIENTED_EDGE('',*,*,#2710,.T.);
#2077=ORIENTED_EDGE('',*,*,#2977,.F.);
#2078=ORIENTED_EDGE('',*,*,#2977,.T.);
#2079=ORIENTED_EDGE('',*,*,#2976,.F.);
#2080=ORIENTED_EDGE('',*,*,#2708,.F.);
#2081=ORIENTED_EDGE('',*,*,#2978,.F.);
#2082=ORIENTED_EDGE('',*,*,#2979,.T.);
#2083=ORIENTED_EDGE('',*,*,#2980,.T.);
#2084=ORIENTED_EDGE('',*,*,#2979,.F.);
#2085=ORIENTED_EDGE('',*,*,#2975,.T.);
#2086=ORIENTED_EDGE('',*,*,#2980,.F.);
#2087=ORIENTED_EDGE('',*,*,#2978,.T.);
#2088=ORIENTED_EDGE('',*,*,#2981,.F.);
#2089=ORIENTED_EDGE('',*,*,#2982,.F.);
#2090=ORIENTED_EDGE('',*,*,#2983,.T.);
#2091=ORIENTED_EDGE('',*,*,#2984,.T.);
#2092=ORIENTED_EDGE('',*,*,#2985,.F.);
#2093=ORIENTED_EDGE('',*,*,#2986,.F.);
#2094=ORIENTED_EDGE('',*,*,#2987,.T.);
#2095=ORIENTED_EDGE('',*,*,#2982,.T.);
#2096=ORIENTED_EDGE('',*,*,#2988,.F.);
#2097=ORIENTED_EDGE('',*,*,#2989,.F.);
#2098=ORIENTED_EDGE('',*,*,#2990,.T.);
#2099=ORIENTED_EDGE('',*,*,#2986,.T.);
#2100=ORIENTED_EDGE('',*,*,#2991,.F.);
#2101=ORIENTED_EDGE('',*,*,#2984,.F.);
#2102=ORIENTED_EDGE('',*,*,#2992,.T.);
#2103=ORIENTED_EDGE('',*,*,#2989,.T.);
#2104=ORIENTED_EDGE('',*,*,#2993,.T.);
#2105=ORIENTED_EDGE('',*,*,#2983,.F.);
#2106=ORIENTED_EDGE('',*,*,#2987,.F.);
#2107=ORIENTED_EDGE('',*,*,#2990,.F.);
#2108=ORIENTED_EDGE('',*,*,#2992,.F.);
#2109=ORIENTED_EDGE('',*,*,#2994,.F.);
#2110=ORIENTED_EDGE('',*,*,#2981,.T.);
#2111=ORIENTED_EDGE('',*,*,#2991,.T.);
#2112=ORIENTED_EDGE('',*,*,#2988,.T.);
#2113=ORIENTED_EDGE('',*,*,#2985,.T.);
#2114=ORIENTED_EDGE('',*,*,#2993,.F.);
#2115=ORIENTED_EDGE('',*,*,#2994,.T.);
#2116=ORIENTED_EDGE('',*,*,#2995,.F.);
#2117=ORIENTED_EDGE('',*,*,#2996,.T.);
#2118=ORIENTED_EDGE('',*,*,#2997,.F.);
#2119=ORIENTED_EDGE('',*,*,#2998,.F.);
#2120=ORIENTED_EDGE('',*,*,#2999,.F.);
#2121=ORIENTED_EDGE('',*,*,#3000,.T.);
#2122=ORIENTED_EDGE('',*,*,#3001,.F.);
#2123=ORIENTED_EDGE('',*,*,#2996,.F.);
#2124=ORIENTED_EDGE('',*,*,#3002,.F.);
#2125=ORIENTED_EDGE('',*,*,#3003,.T.);
#2126=ORIENTED_EDGE('',*,*,#3004,.F.);
#2127=ORIENTED_EDGE('',*,*,#3000,.F.);
#2128=ORIENTED_EDGE('',*,*,#3005,.F.);
#2129=ORIENTED_EDGE('',*,*,#2998,.T.);
#2130=ORIENTED_EDGE('',*,*,#3006,.F.);
#2131=ORIENTED_EDGE('',*,*,#3003,.F.);
#2132=ORIENTED_EDGE('',*,*,#2997,.T.);
#2133=ORIENTED_EDGE('',*,*,#3001,.T.);
#2134=ORIENTED_EDGE('',*,*,#3004,.T.);
#2135=ORIENTED_EDGE('',*,*,#3006,.T.);
#2136=ORIENTED_EDGE('',*,*,#3007,.F.);
#2137=ORIENTED_EDGE('',*,*,#3008,.F.);
#2138=ORIENTED_EDGE('',*,*,#3009,.F.);
#2139=ORIENTED_EDGE('',*,*,#3010,.F.);
#2140=ORIENTED_EDGE('',*,*,#2995,.T.);
#2141=ORIENTED_EDGE('',*,*,#3005,.T.);
#2142=ORIENTED_EDGE('',*,*,#3002,.T.);
#2143=ORIENTED_EDGE('',*,*,#2999,.T.);
#2144=ORIENTED_EDGE('',*,*,#3011,.F.);
#2145=ORIENTED_EDGE('',*,*,#3012,.F.);
#2146=ORIENTED_EDGE('',*,*,#3013,.F.);
#2147=ORIENTED_EDGE('',*,*,#3014,.F.);
#2148=ORIENTED_EDGE('',*,*,#3011,.T.);
#2149=ORIENTED_EDGE('',*,*,#3015,.T.);
#2150=ORIENTED_EDGE('',*,*,#3007,.T.);
#2151=ORIENTED_EDGE('',*,*,#3016,.F.);
#2152=ORIENTED_EDGE('',*,*,#3017,.F.);
#2153=ORIENTED_EDGE('',*,*,#3012,.T.);
#2154=ORIENTED_EDGE('',*,*,#3016,.T.);
#2155=ORIENTED_EDGE('',*,*,#3010,.T.);
#2156=ORIENTED_EDGE('',*,*,#3013,.T.);
#2157=ORIENTED_EDGE('',*,*,#3017,.T.);
#2158=ORIENTED_EDGE('',*,*,#3009,.T.);
#2159=ORIENTED_EDGE('',*,*,#3018,.F.);
#2160=ORIENTED_EDGE('',*,*,#3015,.F.);
#2161=ORIENTED_EDGE('',*,*,#3014,.T.);
#2162=ORIENTED_EDGE('',*,*,#3018,.T.);
#2163=ORIENTED_EDGE('',*,*,#3008,.T.);
#2164=ORIENTED_EDGE('',*,*,#3019,.F.);
#2165=ORIENTED_EDGE('',*,*,#3020,.T.);
#2166=ORIENTED_EDGE('',*,*,#3021,.T.);
#2167=ORIENTED_EDGE('',*,*,#3022,.T.);
#2168=ORIENTED_EDGE('',*,*,#3023,.T.);
#2169=ORIENTED_EDGE('',*,*,#3024,.F.);
#2170=ORIENTED_EDGE('',*,*,#3025,.F.);
#2171=ORIENTED_EDGE('',*,*,#3026,.F.);
#2172=ORIENTED_EDGE('',*,*,#3027,.F.);
#2173=ORIENTED_EDGE('',*,*,#3028,.F.);
#2174=ORIENTED_EDGE('',*,*,#3029,.T.);
#2175=ORIENTED_EDGE('',*,*,#3030,.T.);
#2176=ORIENTED_EDGE('',*,*,#3025,.T.);
#2177=ORIENTED_EDGE('',*,*,#3031,.F.);
#2178=ORIENTED_EDGE('',*,*,#3020,.F.);
#2179=ORIENTED_EDGE('',*,*,#3032,.T.);
#2180=ORIENTED_EDGE('',*,*,#3028,.T.);
#2181=ORIENTED_EDGE('',*,*,#3033,.F.);
#2182=ORIENTED_EDGE('',*,*,#3021,.F.);
#2183=ORIENTED_EDGE('',*,*,#3031,.T.);
#2184=ORIENTED_EDGE('',*,*,#3027,.T.);
#2185=ORIENTED_EDGE('',*,*,#3034,.F.);
#2186=ORIENTED_EDGE('',*,*,#3022,.F.);
#2187=ORIENTED_EDGE('',*,*,#3033,.T.);
#2188=ORIENTED_EDGE('',*,*,#3026,.T.);
#2189=ORIENTED_EDGE('',*,*,#3032,.F.);
#2190=ORIENTED_EDGE('',*,*,#3023,.F.);
#2191=ORIENTED_EDGE('',*,*,#3034,.T.);
#2192=ORIENTED_EDGE('',*,*,#3019,.T.);
#2193=ORIENTED_EDGE('',*,*,#3029,.F.);
#2194=ORIENTED_EDGE('',*,*,#3024,.T.);
#2195=ORIENTED_EDGE('',*,*,#3030,.F.);
#2196=ORIENTED_EDGE('',*,*,#3035,.F.);
#2197=ORIENTED_EDGE('',*,*,#3036,.T.);
#2198=ORIENTED_EDGE('',*,*,#3036,.F.);
#2199=ORIENTED_EDGE('',*,*,#3037,.T.);
#2200=ORIENTED_EDGE('',*,*,#3037,.F.);
#2201=ORIENTED_EDGE('',*,*,#3038,.T.);
#2202=ORIENTED_EDGE('',*,*,#3038,.F.);
#2203=ORIENTED_EDGE('',*,*,#3039,.T.);
#2204=ORIENTED_EDGE('',*,*,#3040,.T.);
#2205=ORIENTED_EDGE('',*,*,#3039,.F.);
#2206=ORIENTED_EDGE('',*,*,#3041,.T.);
#2207=ORIENTED_EDGE('',*,*,#3042,.T.);
#2208=ORIENTED_EDGE('',*,*,#3043,.T.);
#2209=ORIENTED_EDGE('',*,*,#3044,.T.);
#2210=ORIENTED_EDGE('',*,*,#3045,.T.);
#2211=ORIENTED_EDGE('',*,*,#3046,.T.);
#2212=ORIENTED_EDGE('',*,*,#3046,.F.);
#2213=ORIENTED_EDGE('',*,*,#3035,.T.);
#2214=ORIENTED_EDGE('',*,*,#3047,.T.);
#2215=ORIENTED_EDGE('',*,*,#3041,.F.);
#2216=ORIENTED_EDGE('',*,*,#3042,.F.);
#2217=ORIENTED_EDGE('',*,*,#3040,.F.);
#2218=ORIENTED_EDGE('',*,*,#3048,.F.);
#2219=ORIENTED_EDGE('',*,*,#3047,.F.);
#2220=ORIENTED_EDGE('',*,*,#3049,.T.);
#2221=ORIENTED_EDGE('',*,*,#3048,.T.);
#2222=ORIENTED_EDGE('',*,*,#3050,.F.);
#2223=ORIENTED_EDGE('',*,*,#3049,.F.);
#2224=ORIENTED_EDGE('',*,*,#3045,.F.);
#2225=ORIENTED_EDGE('',*,*,#3043,.F.);
#2226=ORIENTED_EDGE('',*,*,#3044,.F.);
#2227=ORIENTED_EDGE('',*,*,#3050,.T.);
#2228=ORIENTED_EDGE('',*,*,#3051,.T.);
#2229=ORIENTED_EDGE('',*,*,#3052,.T.);
#2230=ORIENTED_EDGE('',*,*,#3053,.T.);
#2231=ORIENTED_EDGE('',*,*,#3054,.T.);
#2232=ORIENTED_EDGE('',*,*,#3055,.T.);
#2233=ORIENTED_EDGE('',*,*,#3056,.T.);
#2234=ORIENTED_EDGE('',*,*,#3057,.T.);
#2235=ORIENTED_EDGE('',*,*,#3058,.T.);
#2236=ORIENTED_EDGE('',*,*,#3059,.T.);
#2237=ORIENTED_EDGE('',*,*,#3060,.T.);
#2238=ORIENTED_EDGE('',*,*,#3061,.T.);
#2239=ORIENTED_EDGE('',*,*,#3062,.F.);
#2240=ORIENTED_EDGE('',*,*,#3063,.F.);
#2241=ORIENTED_EDGE('',*,*,#3064,.F.);
#2242=ORIENTED_EDGE('',*,*,#3065,.F.);
#2243=ORIENTED_EDGE('',*,*,#3066,.F.);
#2244=ORIENTED_EDGE('',*,*,#3067,.F.);
#2245=ORIENTED_EDGE('',*,*,#3068,.F.);
#2246=ORIENTED_EDGE('',*,*,#3069,.F.);
#2247=ORIENTED_EDGE('',*,*,#3070,.F.);
#2248=ORIENTED_EDGE('',*,*,#3071,.F.);
#2249=ORIENTED_EDGE('',*,*,#3072,.F.);
#2250=ORIENTED_EDGE('',*,*,#3073,.F.);
#2251=ORIENTED_EDGE('',*,*,#3074,.T.);
#2252=ORIENTED_EDGE('',*,*,#3063,.T.);
#2253=ORIENTED_EDGE('',*,*,#3075,.F.);
#2254=ORIENTED_EDGE('',*,*,#3051,.F.);
#2255=ORIENTED_EDGE('',*,*,#3076,.T.);
#2256=ORIENTED_EDGE('',*,*,#3073,.T.);
#2257=ORIENTED_EDGE('',*,*,#3077,.F.);
#2258=ORIENTED_EDGE('',*,*,#3052,.F.);
#2259=ORIENTED_EDGE('',*,*,#3075,.T.);
#2260=ORIENTED_EDGE('',*,*,#3072,.T.);
#2261=ORIENTED_EDGE('',*,*,#3078,.F.);
#2262=ORIENTED_EDGE('',*,*,#3053,.F.);
#2263=ORIENTED_EDGE('',*,*,#3077,.T.);
#2264=ORIENTED_EDGE('',*,*,#3071,.T.);
#2265=ORIENTED_EDGE('',*,*,#3079,.F.);
#2266=ORIENTED_EDGE('',*,*,#3054,.F.);
#2267=ORIENTED_EDGE('',*,*,#3078,.T.);
#2268=ORIENTED_EDGE('',*,*,#3070,.T.);
#2269=ORIENTED_EDGE('',*,*,#3080,.F.);
#2270=ORIENTED_EDGE('',*,*,#3055,.F.);
#2271=ORIENTED_EDGE('',*,*,#3079,.T.);
#2272=ORIENTED_EDGE('',*,*,#3069,.T.);
#2273=ORIENTED_EDGE('',*,*,#3081,.F.);
#2274=ORIENTED_EDGE('',*,*,#3056,.F.);
#2275=ORIENTED_EDGE('',*,*,#3080,.T.);
#2276=ORIENTED_EDGE('',*,*,#3068,.T.);
#2277=ORIENTED_EDGE('',*,*,#3082,.F.);
#2278=ORIENTED_EDGE('',*,*,#3057,.F.);
#2279=ORIENTED_EDGE('',*,*,#3081,.T.);
#2280=ORIENTED_EDGE('',*,*,#3067,.T.);
#2281=ORIENTED_EDGE('',*,*,#3083,.F.);
#2282=ORIENTED_EDGE('',*,*,#3058,.F.);
#2283=ORIENTED_EDGE('',*,*,#3082,.T.);
#2284=ORIENTED_EDGE('',*,*,#3066,.T.);
#2285=ORIENTED_EDGE('',*,*,#3084,.F.);
#2286=ORIENTED_EDGE('',*,*,#3059,.F.);
#2287=ORIENTED_EDGE('',*,*,#3083,.T.);
#2288=ORIENTED_EDGE('',*,*,#3065,.T.);
#2289=ORIENTED_EDGE('',*,*,#3085,.F.);
#2290=ORIENTED_EDGE('',*,*,#3060,.F.);
#2291=ORIENTED_EDGE('',*,*,#3084,.T.);
#2292=ORIENTED_EDGE('',*,*,#3064,.T.);
#2293=ORIENTED_EDGE('',*,*,#3076,.F.);
#2294=ORIENTED_EDGE('',*,*,#3061,.F.);
#2295=ORIENTED_EDGE('',*,*,#3085,.T.);
#2296=ORIENTED_EDGE('',*,*,#3062,.T.);
#2297=ORIENTED_EDGE('',*,*,#3074,.F.);
#2298=ORIENTED_EDGE('',*,*,#3086,.F.);
#2299=ORIENTED_EDGE('',*,*,#3087,.T.);
#2300=ORIENTED_EDGE('',*,*,#3088,.F.);
#2301=ORIENTED_EDGE('',*,*,#3089,.T.);
#2302=ORIENTED_EDGE('',*,*,#3090,.F.);
#2303=ORIENTED_EDGE('',*,*,#3091,.T.);
#2304=ORIENTED_EDGE('',*,*,#3092,.T.);
#2305=ORIENTED_EDGE('',*,*,#3093,.T.);
#2306=ORIENTED_EDGE('',*,*,#3094,.T.);
#2307=ORIENTED_EDGE('',*,*,#3090,.T.);
#2308=ORIENTED_EDGE('',*,*,#3095,.T.);
#2309=ORIENTED_EDGE('',*,*,#3096,.T.);
#2310=ORIENTED_EDGE('',*,*,#3097,.T.);
#2311=ORIENTED_EDGE('',*,*,#3098,.F.);
#2312=ORIENTED_EDGE('',*,*,#3099,.F.);
#2313=ORIENTED_EDGE('',*,*,#3088,.T.);
#2314=ORIENTED_EDGE('',*,*,#3100,.F.);
#2315=ORIENTED_EDGE('',*,*,#3101,.F.);
#2316=ORIENTED_EDGE('',*,*,#3102,.T.);
#2317=ORIENTED_EDGE('',*,*,#3103,.F.);
#2318=ORIENTED_EDGE('',*,*,#3104,.F.);
#2319=ORIENTED_EDGE('',*,*,#3103,.T.);
#2320=ORIENTED_EDGE('',*,*,#3104,.T.);
#2321=ORIENTED_EDGE('',*,*,#3093,.F.);
#2322=ORIENTED_EDGE('',*,*,#3105,.F.);
#2323=ORIENTED_EDGE('',*,*,#3096,.F.);
#2324=ORIENTED_EDGE('',*,*,#3106,.F.);
#2325=ORIENTED_EDGE('',*,*,#3087,.F.);
#2326=ORIENTED_EDGE('',*,*,#3098,.T.);
#2327=ORIENTED_EDGE('',*,*,#3107,.T.);
#2328=ORIENTED_EDGE('',*,*,#3101,.T.);
#2329=ORIENTED_EDGE('',*,*,#3108,.F.);
#2330=ORIENTED_EDGE('',*,*,#3105,.T.);
#2331=ORIENTED_EDGE('',*,*,#3086,.T.);
#2332=ORIENTED_EDGE('',*,*,#3106,.T.);
#2333=ORIENTED_EDGE('',*,*,#3102,.F.);
#2334=ORIENTED_EDGE('',*,*,#3107,.F.);
#2335=ORIENTED_EDGE('',*,*,#3097,.F.);
#2336=ORIENTED_EDGE('',*,*,#3099,.T.);
#2337=ORIENTED_EDGE('',*,*,#3108,.T.);
#2338=ORIENTED_EDGE('',*,*,#3100,.T.);
#2339=ORIENTED_EDGE('',*,*,#3091,.F.);
#2340=ORIENTED_EDGE('',*,*,#3095,.F.);
#2341=ORIENTED_EDGE('',*,*,#3089,.F.);
#2342=ORIENTED_EDGE('',*,*,#3092,.F.);
#2343=ORIENTED_EDGE('',*,*,#3094,.F.);
#2344=EDGE_CURVE('',#3109,#3109,#3650,.T.);
#2345=EDGE_CURVE('',#3110,#3110,#3651,.T.);
#2346=EDGE_CURVE('',#3111,#3111,#790,.T.);
#2347=EDGE_CURVE('',#3112,#3112,#3652,.T.);
#2348=EDGE_CURVE('',#3113,#3113,#3653,.T.);
#2349=EDGE_CURVE('',#3114,#3114,#791,.T.);
#2350=EDGE_CURVE('',#3115,#3115,#3654,.T.);
#2351=EDGE_CURVE('',#3116,#3116,#3655,.T.);
#2352=EDGE_CURVE('',#3117,#3117,#3656,.T.);
#2353=EDGE_CURVE('',#3118,#3118,#3657,.T.);
#2354=EDGE_CURVE('',#3119,#3119,#3658,.T.);
#2355=EDGE_CURVE('',#3120,#3120,#3659,.T.);
#2356=EDGE_CURVE('',#3121,#3121,#3660,.T.);
#2357=EDGE_CURVE('',#3122,#3122,#3661,.T.);
#2358=EDGE_CURVE('',#3123,#3123,#3662,.T.);
#2359=EDGE_CURVE('',#3124,#3124,#3663,.T.);
#2360=EDGE_CURVE('',#3125,#3126,#35,.T.);
#2361=EDGE_CURVE('',#3125,#3126,#3664,.F.);
#2362=EDGE_CURVE('',#3127,#3128,#3665,.F.);
#2363=EDGE_CURVE('',#3127,#3129,#792,.T.);
#2364=EDGE_CURVE('',#3130,#3129,#3666,.F.);
#2365=EDGE_CURVE('',#3130,#3128,#793,.T.);
#2366=EDGE_CURVE('',#3131,#3131,#3667,.T.);
#2367=EDGE_CURVE('',#3132,#3132,#3668,.T.);
#2368=EDGE_CURVE('',#3133,#3133,#3669,.F.);
#2369=EDGE_CURVE('',#3129,#3130,#36,.T.);
#2370=EDGE_CURVE('',#3134,#3135,#3670,.F.);
#2371=EDGE_CURVE('',#3135,#3136,#794,.T.);
#2372=EDGE_CURVE('',#3137,#3136,#3671,.T.);
#2373=EDGE_CURVE('',#3127,#3137,#795,.T.);
#2374=EDGE_CURVE('',#3138,#3128,#796,.T.);
#2375=EDGE_CURVE('',#3139,#3138,#3672,.T.);
#2376=EDGE_CURVE('',#3139,#3134,#797,.T.);
#2377=EDGE_CURVE('',#3140,#3140,#3673,.T.);
#2378=EDGE_CURVE('',#3141,#3141,#3674,.T.);
#2379=EDGE_CURVE('',#3135,#3125,#798,.T.);
#2380=EDGE_CURVE('',#3126,#3134,#799,.T.);
#2381=EDGE_CURVE('',#3136,#3139,#37,.T.);
#2382=EDGE_CURVE('',#3137,#3138,#38,.T.);
#2383=EDGE_CURVE('',#3142,#3143,#3675,.T.);
#2384=EDGE_CURVE('',#3144,#3143,#39,.T.);
#2385=EDGE_CURVE('',#3145,#3144,#3676,.T.);
#2386=EDGE_CURVE('',#3145,#3142,#40,.T.);
#2387=EDGE_CURVE('',#3146,#3147,#3677,.T.);
#2388=EDGE_CURVE('',#3148,#3146,#41,.F.);
#2389=EDGE_CURVE('',#3148,#3149,#3678,.T.);
#2390=EDGE_CURVE('',#3147,#3149,#42,.T.);
#2391=EDGE_CURVE('',#3150,#3150,#3679,.T.);
#2392=EDGE_CURVE('',#3151,#3151,#3680,.T.);
#2393=EDGE_CURVE('',#3152,#3153,#43,.T.);
#2394=EDGE_CURVE('',#3154,#3152,#3681,.T.);
#2395=EDGE_CURVE('',#3155,#3154,#44,.T.);
#2396=EDGE_CURVE('',#3153,#3155,#3682,.T.);
#2397=EDGE_CURVE('',#3156,#3144,#3683,.T.);
#2398=EDGE_CURVE('',#3157,#3156,#3684,.T.);
#2399=EDGE_CURVE('',#3158,#3157,#3685,.T.);
#2400=EDGE_CURVE('',#3158,#3159,#3686,.T.);
#2401=EDGE_CURVE('',#3160,#3159,#3687,.T.);
#2402=EDGE_CURVE('',#3161,#3160,#3688,.T.);
#2403=EDGE_CURVE('',#3162,#3161,#3689,.T.);
#2404=EDGE_CURVE('',#3162,#3163,#3690,.T.);
#2405=EDGE_CURVE('',#3164,#3163,#3691,.T.);
#2406=EDGE_CURVE('',#3165,#3164,#3692,.T.);
#2407=EDGE_CURVE('',#3166,#3165,#3693,.T.);
#2408=EDGE_CURVE('',#3166,#3167,#3694,.T.);
#2409=EDGE_CURVE('',#3168,#3167,#3695,.T.);
#2410=EDGE_CURVE('',#3169,#3168,#3696,.T.);
#2411=EDGE_CURVE('',#3170,#3169,#3697,.T.);
#2412=EDGE_CURVE('',#3170,#3171,#3698,.T.);
#2413=EDGE_CURVE('',#3172,#3171,#3699,.T.);
#2414=EDGE_CURVE('',#3173,#3172,#3700,.T.);
#2415=EDGE_CURVE('',#3174,#3173,#3701,.T.);
#2416=EDGE_CURVE('',#3174,#3175,#3702,.T.);
#2417=EDGE_CURVE('',#3176,#3175,#3703,.T.);
#2418=EDGE_CURVE('',#3177,#3176,#3704,.T.);
#2419=EDGE_CURVE('',#3178,#3177,#3705,.T.);
#2420=EDGE_CURVE('',#3178,#3179,#3706,.T.);
#2421=EDGE_CURVE('',#3180,#3179,#3707,.T.);
#2422=EDGE_CURVE('',#3181,#3180,#3708,.T.);
#2423=EDGE_CURVE('',#3182,#3181,#3709,.T.);
#2424=EDGE_CURVE('',#3182,#3183,#3710,.T.);
#2425=EDGE_CURVE('',#3184,#3183,#3711,.T.);
#2426=EDGE_CURVE('',#3185,#3184,#3712,.T.);
#2427=EDGE_CURVE('',#3186,#3185,#3713,.T.);
#2428=EDGE_CURVE('',#3186,#3187,#3714,.T.);
#2429=EDGE_CURVE('',#3188,#3187,#3715,.T.);
#2430=EDGE_CURVE('',#3189,#3188,#3716,.T.);
#2431=EDGE_CURVE('',#3190,#3189,#3717,.T.);
#2432=EDGE_CURVE('',#3190,#3191,#3718,.T.);
#2433=EDGE_CURVE('',#3192,#3191,#3719,.T.);
#2434=EDGE_CURVE('',#3193,#3192,#3720,.T.);
#2435=EDGE_CURVE('',#3194,#3193,#3721,.T.);
#2436=EDGE_CURVE('',#3194,#3195,#3722,.T.);
#2437=EDGE_CURVE('',#3196,#3195,#3723,.T.);
#2438=EDGE_CURVE('',#3197,#3196,#3724,.T.);
#2439=EDGE_CURVE('',#3146,#3197,#3725,.T.);
#2440=EDGE_CURVE('',#3147,#3198,#45,.T.);
#2441=EDGE_CURVE('',#3198,#3199,#3726,.T.);
#2442=EDGE_CURVE('',#3199,#3200,#46,.T.);
#2443=EDGE_CURVE('',#3200,#3201,#3727,.T.);
#2444=EDGE_CURVE('',#3201,#3202,#47,.T.);
#2445=EDGE_CURVE('',#3202,#3203,#3728,.T.);
#2446=EDGE_CURVE('',#3203,#3145,#3729,.T.);
#2447=EDGE_CURVE('',#3143,#3204,#3730,.T.);
#2448=EDGE_CURVE('',#3205,#3142,#3731,.T.);
#2449=EDGE_CURVE('',#3206,#3205,#3732,.T.);
#2450=EDGE_CURVE('',#3207,#3206,#48,.T.);
#2451=EDGE_CURVE('',#3208,#3207,#3733,.T.);
#2452=EDGE_CURVE('',#3209,#3208,#49,.T.);
#2453=EDGE_CURVE('',#3210,#3209,#3734,.T.);
#2454=EDGE_CURVE('',#3149,#3210,#50,.T.);
#2455=EDGE_CURVE('',#3211,#3148,#3735,.T.);
#2456=EDGE_CURVE('',#3212,#3211,#3736,.T.);
#2457=EDGE_CURVE('',#3213,#3212,#3737,.T.);
#2458=EDGE_CURVE('',#3214,#3213,#3738,.T.);
#2459=EDGE_CURVE('',#3215,#3214,#3739,.T.);
#2460=EDGE_CURVE('',#3216,#3215,#3740,.T.);
#2461=EDGE_CURVE('',#3217,#3216,#3741,.T.);
#2462=EDGE_CURVE('',#3218,#3217,#3742,.T.);
#2463=EDGE_CURVE('',#3219,#3218,#3743,.T.);
#2464=EDGE_CURVE('',#3220,#3219,#3744,.T.);
#2465=EDGE_CURVE('',#3221,#3220,#3745,.T.);
#2466=EDGE_CURVE('',#3222,#3221,#3746,.T.);
#2467=EDGE_CURVE('',#3223,#3222,#3747,.T.);
#2468=EDGE_CURVE('',#3224,#3223,#3748,.T.);
#2469=EDGE_CURVE('',#3225,#3224,#3749,.T.);
#2470=EDGE_CURVE('',#3226,#3225,#3750,.T.);
#2471=EDGE_CURVE('',#3227,#3226,#3751,.T.);
#2472=EDGE_CURVE('',#3228,#3227,#3752,.T.);
#2473=EDGE_CURVE('',#3229,#3228,#3753,.T.);
#2474=EDGE_CURVE('',#3230,#3229,#3754,.T.);
#2475=EDGE_CURVE('',#3231,#3230,#3755,.T.);
#2476=EDGE_CURVE('',#3232,#3231,#3756,.T.);
#2477=EDGE_CURVE('',#3233,#3232,#3757,.T.);
#2478=EDGE_CURVE('',#3234,#3233,#3758,.T.);
#2479=EDGE_CURVE('',#3235,#3234,#3759,.T.);
#2480=EDGE_CURVE('',#3236,#3235,#3760,.T.);
#2481=EDGE_CURVE('',#3237,#3236,#3761,.T.);
#2482=EDGE_CURVE('',#3238,#3237,#3762,.T.);
#2483=EDGE_CURVE('',#3239,#3238,#3763,.T.);
#2484=EDGE_CURVE('',#3240,#3239,#3764,.T.);
#2485=EDGE_CURVE('',#3241,#3240,#3765,.T.);
#2486=EDGE_CURVE('',#3242,#3241,#3766,.T.);
#2487=EDGE_CURVE('',#3243,#3242,#3767,.T.);
#2488=EDGE_CURVE('',#3244,#3243,#3768,.T.);
#2489=EDGE_CURVE('',#3245,#3244,#3769,.T.);
#2490=EDGE_CURVE('',#3246,#3245,#3770,.T.);
#2491=EDGE_CURVE('',#3247,#3246,#3771,.T.);
#2492=EDGE_CURVE('',#3248,#3247,#3772,.T.);
#2493=EDGE_CURVE('',#3249,#3248,#3773,.T.);
#2494=EDGE_CURVE('',#3250,#3249,#3774,.T.);
#2495=EDGE_CURVE('',#3251,#3250,#3775,.T.);
#2496=EDGE_CURVE('',#3204,#3251,#3776,.T.);
#2497=EDGE_CURVE('',#3252,#3253,#3777,.T.);
#2498=EDGE_CURVE('',#3253,#3254,#51,.T.);
#2499=EDGE_CURVE('',#3254,#3255,#3778,.T.);
#2500=EDGE_CURVE('',#3255,#3252,#52,.T.);
#2501=EDGE_CURVE('',#3198,#3210,#53,.T.);
#2502=EDGE_CURVE('',#3203,#3205,#54,.T.);
#2503=EDGE_CURVE('',#3202,#3206,#55,.T.);
#2504=EDGE_CURVE('',#3201,#3207,#56,.T.);
#2505=EDGE_CURVE('',#3200,#3208,#57,.T.);
#2506=EDGE_CURVE('',#3199,#3209,#58,.T.);
#2507=EDGE_CURVE('',#3154,#3252,#59,.T.);
#2508=EDGE_CURVE('',#3152,#3253,#60,.T.);
#2509=EDGE_CURVE('',#3153,#3254,#61,.T.);
#2510=EDGE_CURVE('',#3155,#3255,#62,.T.);
#2511=EDGE_CURVE('',#3214,#3194,#63,.F.);
#2512=EDGE_CURVE('',#3195,#3213,#64,.T.);
#2513=EDGE_CURVE('',#3218,#3190,#65,.F.);
#2514=EDGE_CURVE('',#3191,#3217,#66,.T.);
#2515=EDGE_CURVE('',#3187,#3221,#67,.T.);
#2516=EDGE_CURVE('',#3222,#3186,#68,.F.);
#2517=EDGE_CURVE('',#3183,#3225,#69,.T.);
#2518=EDGE_CURVE('',#3226,#3182,#70,.F.);
#2519=EDGE_CURVE('',#3230,#3178,#71,.F.);
#2520=EDGE_CURVE('',#3179,#3229,#72,.T.);
#2521=EDGE_CURVE('',#3234,#3174,#73,.F.);
#2522=EDGE_CURVE('',#3175,#3233,#74,.T.);
#2523=EDGE_CURVE('',#3171,#3237,#75,.T.);
#2524=EDGE_CURVE('',#3238,#3170,#76,.F.);
#2525=EDGE_CURVE('',#3242,#3166,#77,.F.);
#2526=EDGE_CURVE('',#3167,#3241,#78,.T.);
#2527=EDGE_CURVE('',#3246,#3162,#79,.F.);
#2528=EDGE_CURVE('',#3163,#3245,#80,.T.);
#2529=EDGE_CURVE('',#3250,#3158,#81,.F.);
#2530=EDGE_CURVE('',#3159,#3249,#82,.T.);
#2531=EDGE_CURVE('',#3156,#3204,#83,.T.);
#2532=EDGE_CURVE('',#3157,#3251,#84,.T.);
#2533=EDGE_CURVE('',#3160,#3248,#85,.T.);
#2534=EDGE_CURVE('',#3161,#3247,#86,.T.);
#2535=EDGE_CURVE('',#3164,#3244,#87,.T.);
#2536=EDGE_CURVE('',#3165,#3243,#88,.T.);
#2537=EDGE_CURVE('',#3168,#3240,#89,.T.);
#2538=EDGE_CURVE('',#3169,#3239,#90,.T.);
#2539=EDGE_CURVE('',#3172,#3236,#91,.T.);
#2540=EDGE_CURVE('',#3173,#3235,#92,.T.);
#2541=EDGE_CURVE('',#3176,#3232,#93,.T.);
#2542=EDGE_CURVE('',#3177,#3231,#94,.T.);
#2543=EDGE_CURVE('',#3180,#3228,#95,.T.);
#2544=EDGE_CURVE('',#3181,#3227,#96,.T.);
#2545=EDGE_CURVE('',#3184,#3224,#97,.T.);
#2546=EDGE_CURVE('',#3185,#3223,#98,.T.);
#2547=EDGE_CURVE('',#3188,#3220,#99,.T.);
#2548=EDGE_CURVE('',#3189,#3219,#100,.T.);
#2549=EDGE_CURVE('',#3192,#3216,#101,.T.);
#2550=EDGE_CURVE('',#3193,#3215,#102,.T.);
#2551=EDGE_CURVE('',#3196,#3212,#103,.T.);
#2552=EDGE_CURVE('',#3197,#3211,#104,.T.);
#2553=EDGE_CURVE('',#3256,#3257,#105,.F.);
#2554=EDGE_CURVE('',#3257,#3258,#106,.T.);
#2555=EDGE_CURVE('',#3258,#3259,#107,.T.);
#2556=EDGE_CURVE('',#3256,#3259,#108,.T.);
#2557=EDGE_CURVE('',#3260,#3261,#109,.T.);
#2558=EDGE_CURVE('',#3261,#3262,#110,.T.);
#2559=EDGE_CURVE('',#3262,#3263,#111,.F.);
#2560=EDGE_CURVE('',#3263,#3264,#112,.T.);
#2561=EDGE_CURVE('',#3264,#3260,#113,.T.);
#2562=EDGE_CURVE('',#3265,#3266,#114,.T.);
#2563=EDGE_CURVE('',#3265,#3267,#115,.T.);
#2564=EDGE_CURVE('',#3268,#3267,#3779,.T.);
#2565=EDGE_CURVE('',#3269,#3268,#116,.T.);
#2566=EDGE_CURVE('',#3270,#3269,#3780,.T.);
#2567=EDGE_CURVE('',#3270,#3266,#117,.F.);
#2568=EDGE_CURVE('',#3271,#3272,#118,.T.);
#2569=EDGE_CURVE('',#3271,#3273,#119,.F.);
#2570=EDGE_CURVE('',#3274,#3273,#120,.T.);
#2571=EDGE_CURVE('',#3275,#3274,#121,.T.);
#2572=EDGE_CURVE('',#3275,#3272,#122,.T.);
#2573=EDGE_CURVE('',#3276,#3277,#123,.T.);
#2574=EDGE_CURVE('',#3276,#3278,#124,.T.);
#2575=EDGE_CURVE('',#3278,#3279,#125,.T.);
#2576=EDGE_CURVE('',#3279,#3277,#126,.F.);
#2577=EDGE_CURVE('',#3280,#3281,#127,.T.);
#2578=EDGE_CURVE('',#3280,#3282,#128,.F.);
#2579=EDGE_CURVE('',#3283,#3282,#129,.T.);
#2580=EDGE_CURVE('',#3284,#3283,#130,.T.);
#2581=EDGE_CURVE('',#3284,#3281,#131,.T.);
#2582=EDGE_CURVE('',#3285,#3286,#132,.F.);
#2583=EDGE_CURVE('',#3286,#3287,#133,.T.);
#2584=EDGE_CURVE('',#3287,#3288,#134,.T.);
#2585=EDGE_CURVE('',#3285,#3288,#135,.T.);
#2586=EDGE_CURVE('',#3289,#3290,#136,.T.);
#2587=EDGE_CURVE('',#3290,#3291,#137,.T.);
#2588=EDGE_CURVE('',#3291,#3292,#138,.F.);
#2589=EDGE_CURVE('',#3292,#3293,#139,.T.);
#2590=EDGE_CURVE('',#3293,#3289,#140,.T.);
#2591=EDGE_CURVE('',#3265,#3257,#3781,.F.);
#2592=EDGE_CURVE('',#3294,#3256,#3782,.T.);
#2593=EDGE_CURVE('',#3295,#3294,#141,.T.);
#2594=EDGE_CURVE('',#3267,#3295,#800,.T.);
#2595=EDGE_CURVE('',#3262,#3272,#3783,.F.);
#2596=EDGE_CURVE('',#3263,#3275,#3784,.F.);
#2597=EDGE_CURVE('',#3258,#3286,#3785,.F.);
#2598=EDGE_CURVE('',#3259,#3285,#3786,.T.);
#2599=EDGE_CURVE('',#3291,#3261,#3787,.F.);
#2600=EDGE_CURVE('',#3292,#3260,#3788,.F.);
#2601=EDGE_CURVE('',#3287,#3277,#3789,.F.);
#2602=EDGE_CURVE('',#3288,#3279,#3790,.T.);
#2603=EDGE_CURVE('',#3280,#3290,#3791,.F.);
#2604=EDGE_CURVE('',#3282,#3289,#3792,.F.);
#2605=EDGE_CURVE('',#3276,#3266,#3793,.F.);
#2606=EDGE_CURVE('',#3296,#3270,#801,.T.);
#2607=EDGE_CURVE('',#3297,#3296,#142,.F.);
#2608=EDGE_CURVE('',#3278,#3297,#3794,.T.);
#2609=EDGE_CURVE('',#3271,#3281,#3795,.F.);
#2610=EDGE_CURVE('',#3273,#3284,#3796,.F.);
#2611=EDGE_CURVE('',#3294,#3297,#143,.T.);
#2612=EDGE_CURVE('',#3298,#3296,#3797,.T.);
#2613=EDGE_CURVE('',#3299,#3298,#144,.T.);
#2614=EDGE_CURVE('',#3295,#3299,#3798,.T.);
#2615=EDGE_CURVE('',#3274,#3264,#3799,.T.);
#2616=EDGE_CURVE('',#3264,#3293,#3800,.T.);
#2617=EDGE_CURVE('',#3293,#3283,#3801,.T.);
#2618=EDGE_CURVE('',#3300,#3301,#145,.T.);
#2619=EDGE_CURVE('',#3302,#3301,#3802,.F.);
#2620=EDGE_CURVE('',#3303,#3302,#146,.T.);
#2621=EDGE_CURVE('',#3303,#3300,#147,.T.);
#2622=EDGE_CURVE('',#3283,#3274,#3803,.T.);
#2623=EDGE_CURVE('',#3304,#3304,#3804,.F.);
#2624=EDGE_CURVE('',#3305,#3305,#3805,.F.);
#2625=EDGE_CURVE('',#3306,#3306,#3806,.T.);
#2626=EDGE_CURVE('',#3307,#3307,#3807,.T.);
#2627=EDGE_CURVE('',#3308,#3299,#148,.T.);
#2628=EDGE_CURVE('',#3309,#3308,#3808,.T.);
#2629=EDGE_CURVE('',#3309,#3268,#149,.T.);
#2630=EDGE_CURVE('',#3310,#3309,#150,.T.);
#2631=EDGE_CURVE('',#3310,#3311,#3809,.T.);
#2632=EDGE_CURVE('',#3312,#3311,#151,.T.);
#2633=EDGE_CURVE('',#3312,#3269,#152,.T.);
#2634=EDGE_CURVE('',#3313,#3312,#3810,.T.);
#2635=EDGE_CURVE('',#3313,#3298,#153,.T.);
#2636=EDGE_CURVE('',#3308,#3313,#154,.T.);
#2637=EDGE_CURVE('',#3301,#3311,#155,.T.);
#2638=EDGE_CURVE('',#3314,#3300,#3811,.T.);
#2639=EDGE_CURVE('',#3315,#3314,#156,.T.);
#2640=EDGE_CURVE('',#3316,#3315,#3812,.T.);
#2641=EDGE_CURVE('',#3317,#3316,#157,.T.);
#2642=EDGE_CURVE('',#3310,#3317,#158,.F.);
#2643=EDGE_CURVE('',#3318,#3315,#159,.T.);
#2644=EDGE_CURVE('',#3319,#3318,#3813,.T.);
#2645=EDGE_CURVE('',#3319,#3316,#160,.T.);
#2646=EDGE_CURVE('',#3302,#3319,#161,.T.);
#2647=EDGE_CURVE('',#3317,#3302,#3814,.F.);
#2648=EDGE_CURVE('',#3320,#3303,#3815,.T.);
#2649=EDGE_CURVE('',#3320,#3314,#162,.T.);
#2650=EDGE_CURVE('',#3318,#3320,#163,.T.);
#2651=EDGE_CURVE('',#3321,#3321,#3816,.T.);
#2652=EDGE_CURVE('',#3322,#3322,#3817,.T.);
#2653=EDGE_CURVE('',#3323,#3323,#3818,.T.);
#2654=EDGE_CURVE('',#3324,#3324,#3819,.T.);
#2655=EDGE_CURVE('',#3325,#3326,#3820,.T.);
#2656=EDGE_CURVE('',#3326,#3327,#164,.T.);
#2657=EDGE_CURVE('',#3327,#3328,#3821,.T.);
#2658=EDGE_CURVE('',#3328,#3325,#165,.T.);
#2659=EDGE_CURVE('',#3329,#3329,#3822,.T.);
#2660=EDGE_CURVE('',#3330,#3331,#3823,.T.);
#2661=EDGE_CURVE('',#3332,#3330,#166,.T.);
#2662=EDGE_CURVE('',#3333,#3332,#3824,.T.);
#2663=EDGE_CURVE('',#3331,#3333,#167,.T.);
#2664=EDGE_CURVE('',#3334,#3334,#3825,.T.);
#2665=EDGE_CURVE('',#3326,#3331,#168,.T.);
#2666=EDGE_CURVE('',#3325,#3330,#169,.T.);
#2667=EDGE_CURVE('',#3327,#3333,#170,.T.);
#2668=EDGE_CURVE('',#3328,#3332,#171,.T.);
#2669=EDGE_CURVE('',#3335,#3335,#3826,.T.);
#2670=EDGE_CURVE('',#3336,#3336,#3827,.T.);
#2671=EDGE_CURVE('',#3337,#3337,#3828,.F.);
#2672=EDGE_CURVE('',#3338,#3338,#3829,.T.);
#2673=EDGE_CURVE('',#3339,#3339,#3830,.T.);
#2674=EDGE_CURVE('',#3340,#3340,#3831,.F.);
#2675=EDGE_CURVE('',#3341,#3342,#172,.T.);
#2676=EDGE_CURVE('',#3343,#3341,#173,.T.);
#2677=EDGE_CURVE('',#3343,#3344,#174,.T.);
#2678=EDGE_CURVE('',#3344,#3342,#175,.T.);
#2679=EDGE_CURVE('',#3341,#3345,#176,.T.);
#2680=EDGE_CURVE('',#3346,#3345,#177,.T.);
#2681=EDGE_CURVE('',#3343,#3346,#178,.T.);
#2682=EDGE_CURVE('',#3345,#3347,#179,.T.);
#2683=EDGE_CURVE('',#3348,#3347,#180,.T.);
#2684=EDGE_CURVE('',#3346,#3348,#181,.T.);
#2685=EDGE_CURVE('',#3349,#3349,#3832,.T.);
#2686=EDGE_CURVE('',#3350,#3350,#3833,.T.);
#2687=EDGE_CURVE('',#3342,#3347,#182,.T.);
#2688=EDGE_CURVE('',#3344,#3348,#183,.T.);
#2689=EDGE_CURVE('',#3351,#3351,#3834,.T.);
#2690=EDGE_CURVE('',#3352,#3352,#3835,.T.);
#2691=EDGE_CURVE('',#3353,#3353,#3836,.T.);
#2692=EDGE_CURVE('',#3354,#3354,#3837,.T.);
#2693=EDGE_CURVE('',#3355,#3355,#3838,.F.);
#2694=EDGE_CURVE('',#3356,#3356,#3839,.F.);
#2695=EDGE_CURVE('',#3357,#3357,#3840,.F.);
#2696=EDGE_CURVE('',#3358,#3358,#3841,.F.);
#2697=EDGE_CURVE('',#3359,#3359,#3842,.T.);
#2698=EDGE_CURVE('',#3360,#3360,#3843,.T.);
#2699=EDGE_CURVE('',#3361,#3361,#3844,.T.);
#2700=EDGE_CURVE('',#3362,#3362,#3845,.T.);
#2701=EDGE_CURVE('',#3363,#3363,#3846,.T.);
#2702=EDGE_CURVE('',#3364,#3364,#3847,.T.);
#2703=EDGE_CURVE('',#3365,#3365,#3848,.T.);
#2704=EDGE_CURVE('',#3366,#3366,#3849,.T.);
#2705=EDGE_CURVE('',#3367,#3367,#3850,.T.);
#2706=EDGE_CURVE('',#3368,#3368,#3851,.T.);
#2707=EDGE_CURVE('',#3369,#3369,#3852,.F.);
#2708=EDGE_CURVE('',#3370,#3370,#3853,.T.);
#2709=EDGE_CURVE('',#3371,#3371,#3854,.F.);
#2710=EDGE_CURVE('',#3372,#3372,#3855,.T.);
#2711=EDGE_CURVE('',#3373,#3374,#3856,.T.);
#2712=EDGE_CURVE('',#3375,#3373,#3857,.T.);
#2713=EDGE_CURVE('',#3376,#3375,#3858,.T.);
#2714=EDGE_CURVE('',#3377,#3376,#3859,.T.);
#2715=EDGE_CURVE('',#3378,#3377,#3860,.T.);
#2716=EDGE_CURVE('',#3379,#3378,#3861,.T.);
#2717=EDGE_CURVE('',#3380,#3379,#3862,.T.);
#2718=EDGE_CURVE('',#3381,#3380,#3863,.T.);
#2719=EDGE_CURVE('',#3382,#3381,#3864,.T.);
#2720=EDGE_CURVE('',#3383,#3382,#3865,.T.);
#2721=EDGE_CURVE('',#3384,#3383,#3866,.T.);
#2722=EDGE_CURVE('',#3385,#3384,#3867,.T.);
#2723=EDGE_CURVE('',#3386,#3385,#3868,.T.);
#2724=EDGE_CURVE('',#3387,#3386,#3869,.T.);
#2725=EDGE_CURVE('',#3388,#3387,#3870,.T.);
#2726=EDGE_CURVE('',#3389,#3388,#3871,.T.);
#2727=EDGE_CURVE('',#3390,#3389,#3872,.T.);
#2728=EDGE_CURVE('',#3391,#3390,#3873,.T.);
#2729=EDGE_CURVE('',#3392,#3391,#3874,.T.);
#2730=EDGE_CURVE('',#3393,#3392,#3875,.T.);
#2731=EDGE_CURVE('',#3394,#3393,#3876,.T.);
#2732=EDGE_CURVE('',#3395,#3394,#3877,.T.);
#2733=EDGE_CURVE('',#3396,#3395,#3878,.T.);
#2734=EDGE_CURVE('',#3397,#3396,#3879,.T.);
#2735=EDGE_CURVE('',#3398,#3397,#3880,.T.);
#2736=EDGE_CURVE('',#3399,#3398,#3881,.T.);
#2737=EDGE_CURVE('',#3400,#3399,#3882,.T.);
#2738=EDGE_CURVE('',#3401,#3400,#3883,.T.);
#2739=EDGE_CURVE('',#3402,#3401,#3884,.T.);
#2740=EDGE_CURVE('',#3403,#3402,#3885,.T.);
#2741=EDGE_CURVE('',#3404,#3403,#3886,.T.);
#2742=EDGE_CURVE('',#3405,#3404,#3887,.T.);
#2743=EDGE_CURVE('',#3406,#3405,#3888,.T.);
#2744=EDGE_CURVE('',#3407,#3406,#3889,.T.);
#2745=EDGE_CURVE('',#3408,#3407,#3890,.T.);
#2746=EDGE_CURVE('',#3409,#3408,#3891,.T.);
#2747=EDGE_CURVE('',#3410,#3409,#3892,.T.);
#2748=EDGE_CURVE('',#3411,#3410,#3893,.T.);
#2749=EDGE_CURVE('',#3412,#3411,#3894,.T.);
#2750=EDGE_CURVE('',#3413,#3412,#3895,.T.);
#2751=EDGE_CURVE('',#3414,#3413,#3896,.T.);
#2752=EDGE_CURVE('',#3415,#3414,#3897,.T.);
#2753=EDGE_CURVE('',#3416,#3415,#3898,.T.);
#2754=EDGE_CURVE('',#3417,#3416,#3899,.T.);
#2755=EDGE_CURVE('',#3418,#3417,#3900,.T.);
#2756=EDGE_CURVE('',#3419,#3418,#3901,.T.);
#2757=EDGE_CURVE('',#3420,#3419,#3902,.T.);
#2758=EDGE_CURVE('',#3421,#3420,#3903,.T.);
#2759=EDGE_CURVE('',#3422,#3421,#3904,.T.);
#2760=EDGE_CURVE('',#3423,#3422,#3905,.T.);
#2761=EDGE_CURVE('',#3424,#3423,#3906,.T.);
#2762=EDGE_CURVE('',#3425,#3424,#3907,.T.);
#2763=EDGE_CURVE('',#3426,#3425,#3908,.T.);
#2764=EDGE_CURVE('',#3427,#3426,#3909,.T.);
#2765=EDGE_CURVE('',#3428,#3427,#3910,.T.);
#2766=EDGE_CURVE('',#3429,#3428,#3911,.T.);
#2767=EDGE_CURVE('',#3430,#3429,#3912,.T.);
#2768=EDGE_CURVE('',#3431,#3430,#3913,.T.);
#2769=EDGE_CURVE('',#3432,#3431,#3914,.T.);
#2770=EDGE_CURVE('',#3433,#3432,#3915,.T.);
#2771=EDGE_CURVE('',#3434,#3433,#3916,.T.);
#2772=EDGE_CURVE('',#3435,#3434,#3917,.T.);
#2773=EDGE_CURVE('',#3436,#3435,#3918,.T.);
#2774=EDGE_CURVE('',#3437,#3436,#3919,.T.);
#2775=EDGE_CURVE('',#3438,#3437,#3920,.T.);
#2776=EDGE_CURVE('',#3439,#3438,#3921,.T.);
#2777=EDGE_CURVE('',#3440,#3439,#3922,.T.);
#2778=EDGE_CURVE('',#3441,#3440,#3923,.T.);
#2779=EDGE_CURVE('',#3442,#3441,#3924,.T.);
#2780=EDGE_CURVE('',#3443,#3442,#3925,.T.);
#2781=EDGE_CURVE('',#3444,#3443,#3926,.T.);
#2782=EDGE_CURVE('',#3445,#3444,#3927,.T.);
#2783=EDGE_CURVE('',#3446,#3445,#3928,.T.);
#2784=EDGE_CURVE('',#3447,#3446,#3929,.T.);
#2785=EDGE_CURVE('',#3448,#3447,#3930,.T.);
#2786=EDGE_CURVE('',#3449,#3448,#3931,.T.);
#2787=EDGE_CURVE('',#3450,#3449,#3932,.T.);
#2788=EDGE_CURVE('',#3451,#3450,#3933,.T.);
#2789=EDGE_CURVE('',#3452,#3451,#3934,.T.);
#2790=EDGE_CURVE('',#3453,#3452,#3935,.T.);
#2791=EDGE_CURVE('',#3454,#3453,#3936,.T.);
#2792=EDGE_CURVE('',#3455,#3454,#3937,.T.);
#2793=EDGE_CURVE('',#3456,#3455,#3938,.T.);
#2794=EDGE_CURVE('',#3457,#3456,#3939,.T.);
#2795=EDGE_CURVE('',#3458,#3457,#3940,.T.);
#2796=EDGE_CURVE('',#3459,#3458,#3941,.T.);
#2797=EDGE_CURVE('',#3460,#3459,#3942,.T.);
#2798=EDGE_CURVE('',#3374,#3460,#3943,.T.);
#2799=EDGE_CURVE('',#3374,#3461,#184,.T.);
#2800=EDGE_CURVE('',#3462,#3460,#185,.F.);
#2801=EDGE_CURVE('',#3461,#3462,#3944,.T.);
#2802=EDGE_CURVE('',#3463,#3376,#186,.F.);
#2803=EDGE_CURVE('',#3464,#3463,#3945,.T.);
#2804=EDGE_CURVE('',#3377,#3464,#187,.T.);
#2805=EDGE_CURVE('',#3457,#3465,#188,.T.);
#2806=EDGE_CURVE('',#3466,#3456,#189,.F.);
#2807=EDGE_CURVE('',#3465,#3466,#3946,.T.);
#2808=EDGE_CURVE('',#3453,#3467,#190,.T.);
#2809=EDGE_CURVE('',#3468,#3452,#191,.F.);
#2810=EDGE_CURVE('',#3467,#3468,#3947,.T.);
#2811=EDGE_CURVE('',#3445,#3469,#192,.T.);
#2812=EDGE_CURVE('',#3470,#3444,#193,.F.);
#2813=EDGE_CURVE('',#3469,#3470,#3948,.T.);
#2814=EDGE_CURVE('',#3471,#3448,#194,.F.);
#2815=EDGE_CURVE('',#3472,#3471,#3949,.T.);
#2816=EDGE_CURVE('',#3449,#3472,#195,.T.);
#2817=EDGE_CURVE('',#3393,#3473,#196,.T.);
#2818=EDGE_CURVE('',#3474,#3392,#197,.F.);
#2819=EDGE_CURVE('',#3473,#3474,#3950,.T.);
#2820=EDGE_CURVE('',#3475,#3396,#198,.F.);
#2821=EDGE_CURVE('',#3476,#3475,#3951,.T.);
#2822=EDGE_CURVE('',#3397,#3476,#199,.T.);
#2823=EDGE_CURVE('',#3389,#3477,#200,.T.);
#2824=EDGE_CURVE('',#3478,#3388,#201,.F.);
#2825=EDGE_CURVE('',#3477,#3478,#3952,.T.);
#2826=EDGE_CURVE('',#3385,#3479,#202,.T.);
#2827=EDGE_CURVE('',#3480,#3384,#203,.F.);
#2828=EDGE_CURVE('',#3479,#3480,#3953,.T.);
#2829=EDGE_CURVE('',#3481,#3380,#204,.F.);
#2830=EDGE_CURVE('',#3482,#3481,#3954,.T.);
#2831=EDGE_CURVE('',#3381,#3482,#205,.T.);
#2832=EDGE_CURVE('',#3405,#3483,#206,.T.);
#2833=EDGE_CURVE('',#3484,#3404,#207,.F.);
#2834=EDGE_CURVE('',#3483,#3484,#3955,.T.);
#2835=EDGE_CURVE('',#3485,#3408,#208,.F.);
#2836=EDGE_CURVE('',#3486,#3485,#3956,.T.);
#2837=EDGE_CURVE('',#3409,#3486,#209,.T.);
#2838=EDGE_CURVE('',#3487,#3412,#210,.F.);
#2839=EDGE_CURVE('',#3488,#3487,#3957,.T.);
#2840=EDGE_CURVE('',#3413,#3488,#211,.T.);
#2841=EDGE_CURVE('',#3489,#3416,#212,.F.);
#2842=EDGE_CURVE('',#3490,#3489,#3958,.T.);
#2843=EDGE_CURVE('',#3417,#3490,#213,.T.);
#2844=EDGE_CURVE('',#3401,#3491,#214,.T.);
#2845=EDGE_CURVE('',#3492,#3400,#215,.F.);
#2846=EDGE_CURVE('',#3491,#3492,#3959,.T.);
#2847=EDGE_CURVE('',#3425,#3493,#216,.T.);
#2848=EDGE_CURVE('',#3494,#3424,#217,.F.);
#2849=EDGE_CURVE('',#3493,#3494,#3960,.T.);
#2850=EDGE_CURVE('',#3495,#3428,#218,.F.);
#2851=EDGE_CURVE('',#3496,#3495,#3961,.T.);
#2852=EDGE_CURVE('',#3429,#3496,#219,.T.);
#2853=EDGE_CURVE('',#3497,#3432,#220,.F.);
#2854=EDGE_CURVE('',#3498,#3497,#3962,.T.);
#2855=EDGE_CURVE('',#3433,#3498,#221,.T.);
#2856=EDGE_CURVE('',#3499,#3436,#222,.F.);
#2857=EDGE_CURVE('',#3500,#3499,#3963,.T.);
#2858=EDGE_CURVE('',#3437,#3500,#223,.T.);
#2859=EDGE_CURVE('',#3421,#3501,#224,.T.);
#2860=EDGE_CURVE('',#3502,#3420,#225,.F.);
#2861=EDGE_CURVE('',#3501,#3502,#3964,.T.);
#2862=EDGE_CURVE('',#3503,#3461,#3965,.T.);
#2863=EDGE_CURVE('',#3504,#3462,#3966,.T.);
#2864=EDGE_CURVE('',#3504,#3505,#3967,.T.);
#2865=EDGE_CURVE('',#3505,#3465,#3968,.T.);
#2866=EDGE_CURVE('',#3506,#3466,#3969,.T.);
#2867=EDGE_CURVE('',#3506,#3507,#3970,.T.);
#2868=EDGE_CURVE('',#3507,#3467,#3971,.T.);
#2869=EDGE_CURVE('',#3508,#3468,#3972,.T.);
#2870=EDGE_CURVE('',#3508,#3509,#3973,.T.);
#2871=EDGE_CURVE('',#3509,#3472,#3974,.T.);
#2872=EDGE_CURVE('',#3510,#3471,#3975,.T.);
#2873=EDGE_CURVE('',#3510,#3511,#3976,.T.);
#2874=EDGE_CURVE('',#3511,#3469,#3977,.T.);
#2875=EDGE_CURVE('',#3512,#3470,#3978,.T.);
#2876=EDGE_CURVE('',#3512,#3513,#3979,.T.);
#2877=EDGE_CURVE('',#3513,#3514,#3980,.T.);
#2878=EDGE_CURVE('',#3514,#3515,#3981,.T.);
#2879=EDGE_CURVE('',#3516,#3515,#3982,.T.);
#2880=EDGE_CURVE('',#3516,#3517,#3983,.T.);
#2881=EDGE_CURVE('',#3517,#3500,#3984,.T.);
#2882=EDGE_CURVE('',#3518,#3499,#3985,.T.);
#2883=EDGE_CURVE('',#3518,#3519,#3986,.T.);
#2884=EDGE_CURVE('',#3519,#3498,#3987,.T.);
#2885=EDGE_CURVE('',#3520,#3497,#3988,.T.);
#2886=EDGE_CURVE('',#3520,#3521,#3989,.T.);
#2887=EDGE_CURVE('',#3521,#3496,#3990,.T.);
#2888=EDGE_CURVE('',#3522,#3495,#3991,.T.);
#2889=EDGE_CURVE('',#3522,#3523,#3992,.T.);
#2890=EDGE_CURVE('',#3523,#3493,#3993,.T.);
#2891=EDGE_CURVE('',#3524,#3494,#3994,.T.);
#2892=EDGE_CURVE('',#3524,#3525,#3995,.T.);
#2893=EDGE_CURVE('',#3525,#3501,#3996,.T.);
#2894=EDGE_CURVE('',#3526,#3502,#3997,.T.);
#2895=EDGE_CURVE('',#3526,#3527,#3998,.T.);
#2896=EDGE_CURVE('',#3527,#3490,#3999,.T.);
#2897=EDGE_CURVE('',#3528,#3489,#4000,.T.);
#2898=EDGE_CURVE('',#3528,#3529,#4001,.T.);
#2899=EDGE_CURVE('',#3529,#3488,#4002,.T.);
#2900=EDGE_CURVE('',#3530,#3487,#4003,.T.);
#2901=EDGE_CURVE('',#3530,#3531,#4004,.T.);
#2902=EDGE_CURVE('',#3531,#3486,#4005,.T.);
#2903=EDGE_CURVE('',#3532,#3485,#4006,.T.);
#2904=EDGE_CURVE('',#3532,#3533,#4007,.T.);
#2905=EDGE_CURVE('',#3533,#3483,#4008,.T.);
#2906=EDGE_CURVE('',#3534,#3484,#4009,.T.);
#2907=EDGE_CURVE('',#3534,#3535,#4010,.T.);
#2908=EDGE_CURVE('',#3535,#3491,#4011,.T.);
#2909=EDGE_CURVE('',#3536,#3492,#4012,.T.);
#2910=EDGE_CURVE('',#3536,#3537,#4013,.T.);
#2911=EDGE_CURVE('',#3537,#3476,#4014,.T.);
#2912=EDGE_CURVE('',#3538,#3475,#4015,.T.);
#2913=EDGE_CURVE('',#3538,#3539,#4016,.T.);
#2914=EDGE_CURVE('',#3539,#3473,#4017,.T.);
#2915=EDGE_CURVE('',#3540,#3474,#4018,.T.);
#2916=EDGE_CURVE('',#3540,#3541,#4019,.T.);
#2917=EDGE_CURVE('',#3541,#3477,#4020,.T.);
#2918=EDGE_CURVE('',#3542,#3478,#4021,.T.);
#2919=EDGE_CURVE('',#3542,#3543,#4022,.T.);
#2920=EDGE_CURVE('',#3543,#3479,#4023,.T.);
#2921=EDGE_CURVE('',#3544,#3480,#4024,.T.);
#2922=EDGE_CURVE('',#3544,#3545,#4025,.T.);
#2923=EDGE_CURVE('',#3545,#3482,#4026,.T.);
#2924=EDGE_CURVE('',#3546,#3481,#4027,.T.);
#2925=EDGE_CURVE('',#3546,#3547,#4028,.T.);
#2926=EDGE_CURVE('',#3547,#3464,#4029,.T.);
#2927=EDGE_CURVE('',#3548,#3463,#4030,.T.);
#2928=EDGE_CURVE('',#3548,#3503,#4031,.T.);
#2929=EDGE_CURVE('',#3441,#3514,#226,.T.);
#2930=EDGE_CURVE('',#3515,#3440,#227,.F.);
#2931=EDGE_CURVE('',#3438,#3517,#228,.T.);
#2932=EDGE_CURVE('',#3439,#3516,#229,.T.);
#2933=EDGE_CURVE('',#3442,#3513,#230,.T.);
#2934=EDGE_CURVE('',#3443,#3512,#231,.T.);
#2935=EDGE_CURVE('',#3418,#3527,#232,.T.);
#2936=EDGE_CURVE('',#3419,#3526,#233,.T.);
#2937=EDGE_CURVE('',#3422,#3525,#234,.T.);
#2938=EDGE_CURVE('',#3423,#3524,#235,.T.);
#2939=EDGE_CURVE('',#3434,#3519,#236,.T.);
#2940=EDGE_CURVE('',#3435,#3518,#237,.T.);
#2941=EDGE_CURVE('',#3430,#3521,#238,.T.);
#2942=EDGE_CURVE('',#3431,#3520,#239,.T.);
#2943=EDGE_CURVE('',#3426,#3523,#240,.T.);
#2944=EDGE_CURVE('',#3427,#3522,#241,.T.);
#2945=EDGE_CURVE('',#3398,#3537,#242,.T.);
#2946=EDGE_CURVE('',#3399,#3536,#243,.T.);
#2947=EDGE_CURVE('',#3402,#3535,#244,.T.);
#2948=EDGE_CURVE('',#3403,#3534,#245,.T.);
#2949=EDGE_CURVE('',#3414,#3529,#246,.T.);
#2950=EDGE_CURVE('',#3415,#3528,#247,.T.);
#2951=EDGE_CURVE('',#3410,#3531,#248,.T.);
#2952=EDGE_CURVE('',#3411,#3530,#249,.T.);
#2953=EDGE_CURVE('',#3406,#3533,#250,.T.);
#2954=EDGE_CURVE('',#3407,#3532,#251,.T.);
#2955=EDGE_CURVE('',#3382,#3545,#252,.T.);
#2956=EDGE_CURVE('',#3383,#3544,#253,.T.);
#2957=EDGE_CURVE('',#3378,#3547,#254,.T.);
#2958=EDGE_CURVE('',#3379,#3546,#255,.T.);
#2959=EDGE_CURVE('',#3386,#3543,#256,.T.);
#2960=EDGE_CURVE('',#3387,#3542,#257,.T.);
#2961=EDGE_CURVE('',#3390,#3541,#258,.T.);
#2962=EDGE_CURVE('',#3391,#3540,#259,.T.);
#2963=EDGE_CURVE('',#3394,#3539,#260,.T.);
#2964=EDGE_CURVE('',#3395,#3538,#261,.T.);
#2965=EDGE_CURVE('',#3450,#3509,#262,.T.);
#2966=EDGE_CURVE('',#3451,#3508,#263,.T.);
#2967=EDGE_CURVE('',#3446,#3511,#264,.T.);
#2968=EDGE_CURVE('',#3447,#3510,#265,.T.);
#2969=EDGE_CURVE('',#3454,#3507,#266,.T.);
#2970=EDGE_CURVE('',#3455,#3506,#267,.T.);
#2971=EDGE_CURVE('',#3458,#3505,#268,.T.);
#2972=EDGE_CURVE('',#3459,#3504,#269,.T.);
#2973=EDGE_CURVE('',#3373,#3503,#270,.T.);
#2974=EDGE_CURVE('',#3375,#3548,#271,.T.);
#2975=EDGE_CURVE('',#3549,#3549,#4032,.T.);
#2976=EDGE_CURVE('',#3550,#3550,#4033,.T.);
#2977=EDGE_CURVE('',#3551,#3551,#4034,.T.);
#2978=EDGE_CURVE('',#3552,#3552,#4035,.T.);
#2979=EDGE_CURVE('',#3553,#3553,#4036,.T.);
#2980=EDGE_CURVE('',#3554,#3554,#4037,.T.);
#2981=EDGE_CURVE('',#3555,#3556,#4038,.T.);
#2982=EDGE_CURVE('',#3557,#3555,#272,.T.);
#2983=EDGE_CURVE('',#3557,#3558,#4039,.T.);
#2984=EDGE_CURVE('',#3558,#3556,#273,.T.);
#2985=EDGE_CURVE('',#3559,#3555,#4040,.T.);
#2986=EDGE_CURVE('',#3560,#3559,#274,.T.);
#2987=EDGE_CURVE('',#3560,#3557,#4041,.T.);
#2988=EDGE_CURVE('',#3561,#3559,#4042,.T.);
#2989=EDGE_CURVE('',#3562,#3561,#275,.T.);
#2990=EDGE_CURVE('',#3562,#3560,#4043,.T.);
#2991=EDGE_CURVE('',#3556,#3561,#276,.T.);
#2992=EDGE_CURVE('',#3558,#3562,#277,.T.);
#2993=EDGE_CURVE('',#3563,#3563,#4044,.T.);
#2994=EDGE_CURVE('',#3564,#3564,#4045,.T.);
#2995=EDGE_CURVE('',#3565,#3566,#4046,.T.);
#2996=EDGE_CURVE('',#3565,#3567,#4047,.T.);
#2997=EDGE_CURVE('',#3568,#3567,#802,.T.);
#2998=EDGE_CURVE('',#3566,#3568,#4048,.T.);
#2999=EDGE_CURVE('',#3569,#3565,#278,.T.);
#3000=EDGE_CURVE('',#3569,#3570,#4049,.T.);
#3001=EDGE_CURVE('',#3567,#3570,#279,.F.);
#3002=EDGE_CURVE('',#3571,#3569,#4050,.T.);
#3003=EDGE_CURVE('',#3571,#3572,#4051,.T.);
#3004=EDGE_CURVE('',#3570,#3572,#803,.T.);
#3005=EDGE_CURVE('',#3566,#3571,#280,.F.);
#3006=EDGE_CURVE('',#3572,#3568,#281,.T.);
#3007=EDGE_CURVE('',#3573,#3574,#804,.T.);
#3008=EDGE_CURVE('',#3575,#3573,#282,.T.);
#3009=EDGE_CURVE('',#3576,#3575,#805,.T.);
#3010=EDGE_CURVE('',#3574,#3576,#283,.F.);
#3011=EDGE_CURVE('',#3577,#3578,#4052,.T.);
#3012=EDGE_CURVE('',#3579,#3577,#284,.T.);
#3013=EDGE_CURVE('',#3580,#3579,#4053,.T.);
#3014=EDGE_CURVE('',#3578,#3580,#285,.F.);
#3015=EDGE_CURVE('',#3578,#3573,#4054,.T.);
#3016=EDGE_CURVE('',#3577,#3574,#4055,.T.);
#3017=EDGE_CURVE('',#3579,#3576,#4056,.T.);
#3018=EDGE_CURVE('',#3580,#3575,#4057,.T.);
#3019=EDGE_CURVE('',#3581,#3581,#4058,.T.);
#3020=EDGE_CURVE('',#3582,#3583,#4059,.T.);
#3021=EDGE_CURVE('',#3583,#3584,#286,.T.);
#3022=EDGE_CURVE('',#3584,#3585,#4060,.T.);
#3023=EDGE_CURVE('',#3585,#3582,#287,.T.);
#3024=EDGE_CURVE('',#3586,#3586,#4061,.T.);
#3025=EDGE_CURVE('',#3587,#3588,#4062,.T.);
#3026=EDGE_CURVE('',#3589,#3587,#288,.T.);
#3027=EDGE_CURVE('',#3590,#3589,#4063,.T.);
#3028=EDGE_CURVE('',#3588,#3590,#289,.T.);
#3029=EDGE_CURVE('',#3591,#3591,#4064,.T.);
#3030=EDGE_CURVE('',#3592,#3592,#4065,.T.);
#3031=EDGE_CURVE('',#3583,#3588,#290,.T.);
#3032=EDGE_CURVE('',#3582,#3587,#291,.T.);
#3033=EDGE_CURVE('',#3584,#3590,#292,.T.);
#3034=EDGE_CURVE('',#3585,#3589,#293,.T.);
#3035=EDGE_CURVE('',#3593,#3593,#4066,.T.);
#3036=EDGE_CURVE('',#3594,#3594,#4067,.T.);
#3037=EDGE_CURVE('',#3595,#3595,#4068,.T.);
#3038=EDGE_CURVE('',#3596,#3596,#4069,.T.);
#3039=EDGE_CURVE('',#3597,#3597,#4070,.T.);
#3040=EDGE_CURVE('',#3598,#3598,#4071,.T.);
#3041=EDGE_CURVE('',#3599,#3599,#4072,.T.);
#3042=EDGE_CURVE('',#3600,#3600,#4073,.T.);
#3043=EDGE_CURVE('',#3601,#3601,#4074,.T.);
#3044=EDGE_CURVE('',#3602,#3602,#4075,.F.);
#3045=EDGE_CURVE('',#3603,#3603,#4076,.F.);
#3046=EDGE_CURVE('',#3604,#3604,#4077,.T.);
#3047=EDGE_CURVE('',#3605,#3605,#4078,.T.);
#3048=EDGE_CURVE('',#3606,#3606,#4079,.F.);
#3049=EDGE_CURVE('',#3607,#3607,#4080,.T.);
#3050=EDGE_CURVE('',#3608,#3608,#4081,.T.);
#3051=EDGE_CURVE('',#3609,#3610,#4082,.T.);
#3052=EDGE_CURVE('',#3610,#3611,#4083,.T.);
#3053=EDGE_CURVE('',#3611,#3612,#294,.T.);
#3054=EDGE_CURVE('',#3612,#3613,#4084,.T.);
#3055=EDGE_CURVE('',#3613,#3614,#295,.T.);
#3056=EDGE_CURVE('',#3614,#3615,#296,.T.);
#3057=EDGE_CURVE('',#3615,#3616,#4085,.T.);
#3058=EDGE_CURVE('',#3616,#3617,#297,.T.);
#3059=EDGE_CURVE('',#3617,#3618,#4086,.T.);
#3060=EDGE_CURVE('',#3618,#3619,#4087,.T.);
#3061=EDGE_CURVE('',#3619,#3609,#298,.T.);
#3062=EDGE_CURVE('',#3620,#3620,#4088,.T.);
#3063=EDGE_CURVE('',#3621,#3622,#4089,.T.);
#3064=EDGE_CURVE('',#3623,#3621,#299,.T.);
#3065=EDGE_CURVE('',#3624,#3623,#4090,.T.);
#3066=EDGE_CURVE('',#3625,#3624,#4091,.T.);
#3067=EDGE_CURVE('',#3626,#3625,#300,.T.);
#3068=EDGE_CURVE('',#3627,#3626,#4092,.T.);
#3069=EDGE_CURVE('',#3628,#3627,#301,.T.);
#3070=EDGE_CURVE('',#3629,#3628,#302,.T.);
#3071=EDGE_CURVE('',#3630,#3629,#4093,.T.);
#3072=EDGE_CURVE('',#3631,#3630,#303,.T.);
#3073=EDGE_CURVE('',#3622,#3631,#4094,.T.);
#3074=EDGE_CURVE('',#3632,#3632,#4095,.T.);
#3075=EDGE_CURVE('',#3610,#3622,#304,.T.);
#3076=EDGE_CURVE('',#3609,#3621,#305,.T.);
#3077=EDGE_CURVE('',#3611,#3631,#306,.T.);
#3078=EDGE_CURVE('',#3612,#3630,#307,.T.);
#3079=EDGE_CURVE('',#3613,#3629,#308,.T.);
#3080=EDGE_CURVE('',#3614,#3628,#309,.T.);
#3081=EDGE_CURVE('',#3615,#3627,#310,.T.);
#3082=EDGE_CURVE('',#3616,#3626,#311,.T.);
#3083=EDGE_CURVE('',#3617,#3625,#312,.T.);
#3084=EDGE_CURVE('',#3618,#3624,#313,.T.);
#3085=EDGE_CURVE('',#3619,#3623,#314,.T.);
#3086=EDGE_CURVE('',#3633,#3634,#315,.T.);
#3087=EDGE_CURVE('',#3633,#3634,#4096,.F.);
#3088=EDGE_CURVE('',#3635,#3636,#4097,.F.);
#3089=EDGE_CURVE('',#3635,#3637,#806,.T.);
#3090=EDGE_CURVE('',#3638,#3637,#4098,.F.);
#3091=EDGE_CURVE('',#3638,#3636,#807,.T.);
#3092=EDGE_CURVE('',#3639,#3639,#4099,.T.);
#3093=EDGE_CURVE('',#3640,#3640,#4100,.T.);
#3094=EDGE_CURVE('',#3641,#3641,#4101,.F.);
#3095=EDGE_CURVE('',#3637,#3638,#316,.T.);
#3096=EDGE_CURVE('',#3642,#3643,#4102,.F.);
#3097=EDGE_CURVE('',#3643,#3644,#808,.T.);
#3098=EDGE_CURVE('',#3645,#3644,#4103,.T.);
#3099=EDGE_CURVE('',#3635,#3645,#809,.T.);
#3100=EDGE_CURVE('',#3646,#3636,#810,.T.);
#3101=EDGE_CURVE('',#3647,#3646,#4104,.T.);
#3102=EDGE_CURVE('',#3647,#3642,#811,.T.);
#3103=EDGE_CURVE('',#3648,#3648,#4105,.T.);
#3104=EDGE_CURVE('',#3649,#3649,#4106,.T.);
#3105=EDGE_CURVE('',#3643,#3633,#812,.T.);
#3106=EDGE_CURVE('',#3634,#3642,#813,.T.);
#3107=EDGE_CURVE('',#3644,#3647,#317,.T.);
#3108=EDGE_CURVE('',#3645,#3646,#318,.T.);
#3109=VERTEX_POINT('',#8394);
#3110=VERTEX_POINT('',#8396);
#3111=VERTEX_POINT('',#8408);
#3112=VERTEX_POINT('',#8411);
#3113=VERTEX_POINT('',#8413);
#3114=VERTEX_POINT('',#8425);
#3115=VERTEX_POINT('',#8428);
#3116=VERTEX_POINT('',#8431);
#3117=VERTEX_POINT('',#8433);
#3118=VERTEX_POINT('',#8435);
#3119=VERTEX_POINT('',#8437);
#3120=VERTEX_POINT('',#8440);
#3121=VERTEX_POINT('',#8444);
#3122=VERTEX_POINT('',#8446);
#3123=VERTEX_POINT('',#8448);
#3124=VERTEX_POINT('',#8450);
#3125=VERTEX_POINT('',#8459);
#3126=VERTEX_POINT('',#8460);
#3127=VERTEX_POINT('',#8464);
#3128=VERTEX_POINT('',#8465);
#3129=VERTEX_POINT('',#8470);
#3130=VERTEX_POINT('',#8472);
#3131=VERTEX_POINT('',#8479);
#3132=VERTEX_POINT('',#8481);
#3133=VERTEX_POINT('',#8484);
#3134=VERTEX_POINT('',#8489);
#3135=VERTEX_POINT('',#8490);
#3136=VERTEX_POINT('',#8495);
#3137=VERTEX_POINT('',#8497);
#3138=VERTEX_POINT('',#8506);
#3139=VERTEX_POINT('',#8508);
#3140=VERTEX_POINT('',#8514);
#3141=VERTEX_POINT('',#8517);
#3142=VERTEX_POINT('',#8538);
#3143=VERTEX_POINT('',#8539);
#3144=VERTEX_POINT('',#8541);
#3145=VERTEX_POINT('',#8543);
#3146=VERTEX_POINT('',#8547);
#3147=VERTEX_POINT('',#8548);
#3148=VERTEX_POINT('',#8550);
#3149=VERTEX_POINT('',#8552);
#3150=VERTEX_POINT('',#8556);
#3151=VERTEX_POINT('',#8558);
#3152=VERTEX_POINT('',#8561);
#3153=VERTEX_POINT('',#8562);
#3154=VERTEX_POINT('',#8564);
#3155=VERTEX_POINT('',#8566);
#3156=VERTEX_POINT('',#8569);
#3157=VERTEX_POINT('',#8571);
#3158=VERTEX_POINT('',#8573);
#3159=VERTEX_POINT('',#8575);
#3160=VERTEX_POINT('',#8577);
#3161=VERTEX_POINT('',#8579);
#3162=VERTEX_POINT('',#8581);
#3163=VERTEX_POINT('',#8583);
#3164=VERTEX_POINT('',#8585);
#3165=VERTEX_POINT('',#8587);
#3166=VERTEX_POINT('',#8589);
#3167=VERTEX_POINT('',#8591);
#3168=VERTEX_POINT('',#8593);
#3169=VERTEX_POINT('',#8595);
#3170=VERTEX_POINT('',#8597);
#3171=VERTEX_POINT('',#8599);
#3172=VERTEX_POINT('',#8601);
#3173=VERTEX_POINT('',#8603);
#3174=VERTEX_POINT('',#8605);
#3175=VERTEX_POINT('',#8607);
#3176=VERTEX_POINT('',#8609);
#3177=VERTEX_POINT('',#8611);
#3178=VERTEX_POINT('',#8613);
#3179=VERTEX_POINT('',#8615);
#3180=VERTEX_POINT('',#8617);
#3181=VERTEX_POINT('',#8619);
#3182=VERTEX_POINT('',#8621);
#3183=VERTEX_POINT('',#8623);
#3184=VERTEX_POINT('',#8625);
#3185=VERTEX_POINT('',#8627);
#3186=VERTEX_POINT('',#8629);
#3187=VERTEX_POINT('',#8631);
#3188=VERTEX_POINT('',#8633);
#3189=VERTEX_POINT('',#8635);
#3190=VERTEX_POINT('',#8637);
#3191=VERTEX_POINT('',#8639);
#3192=VERTEX_POINT('',#8641);
#3193=VERTEX_POINT('',#8643);
#3194=VERTEX_POINT('',#8645);
#3195=VERTEX_POINT('',#8647);
#3196=VERTEX_POINT('',#8649);
#3197=VERTEX_POINT('',#8651);
#3198=VERTEX_POINT('',#8654);
#3199=VERTEX_POINT('',#8656);
#3200=VERTEX_POINT('',#8658);
#3201=VERTEX_POINT('',#8660);
#3202=VERTEX_POINT('',#8662);
#3203=VERTEX_POINT('',#8664);
#3204=VERTEX_POINT('',#8668);
#3205=VERTEX_POINT('',#8670);
#3206=VERTEX_POINT('',#8672);
#3207=VERTEX_POINT('',#8674);
#3208=VERTEX_POINT('',#8676);
#3209=VERTEX_POINT('',#8678);
#3210=VERTEX_POINT('',#8680);
#3211=VERTEX_POINT('',#8683);
#3212=VERTEX_POINT('',#8685);
#3213=VERTEX_POINT('',#8687);
#3214=VERTEX_POINT('',#8689);
#3215=VERTEX_POINT('',#8691);
#3216=VERTEX_POINT('',#8693);
#3217=VERTEX_POINT('',#8695);
#3218=VERTEX_POINT('',#8697);
#3219=VERTEX_POINT('',#8699);
#3220=VERTEX_POINT('',#8701);
#3221=VERTEX_POINT('',#8703);
#3222=VERTEX_POINT('',#8705);
#3223=VERTEX_POINT('',#8707);
#3224=VERTEX_POINT('',#8709);
#3225=VERTEX_POINT('',#8711);
#3226=VERTEX_POINT('',#8713);
#3227=VERTEX_POINT('',#8715);
#3228=VERTEX_POINT('',#8717);
#3229=VERTEX_POINT('',#8719);
#3230=VERTEX_POINT('',#8721);
#3231=VERTEX_POINT('',#8723);
#3232=VERTEX_POINT('',#8725);
#3233=VERTEX_POINT('',#8727);
#3234=VERTEX_POINT('',#8729);
#3235=VERTEX_POINT('',#8731);
#3236=VERTEX_POINT('',#8733);
#3237=VERTEX_POINT('',#8735);
#3238=VERTEX_POINT('',#8737);
#3239=VERTEX_POINT('',#8739);
#3240=VERTEX_POINT('',#8741);
#3241=VERTEX_POINT('',#8743);
#3242=VERTEX_POINT('',#8745);
#3243=VERTEX_POINT('',#8747);
#3244=VERTEX_POINT('',#8749);
#3245=VERTEX_POINT('',#8751);
#3246=VERTEX_POINT('',#8753);
#3247=VERTEX_POINT('',#8755);
#3248=VERTEX_POINT('',#8757);
#3249=VERTEX_POINT('',#8759);
#3250=VERTEX_POINT('',#8761);
#3251=VERTEX_POINT('',#8763);
#3252=VERTEX_POINT('',#8766);
#3253=VERTEX_POINT('',#8767);
#3254=VERTEX_POINT('',#8769);
#3255=VERTEX_POINT('',#8771);
#3256=VERTEX_POINT('',#8883);
#3257=VERTEX_POINT('',#8884);
#3258=VERTEX_POINT('',#8886);
#3259=VERTEX_POINT('',#8888);
#3260=VERTEX_POINT('',#8892);
#3261=VERTEX_POINT('',#8893);
#3262=VERTEX_POINT('',#8895);
#3263=VERTEX_POINT('',#8897);
#3264=VERTEX_POINT('',#8899);
#3265=VERTEX_POINT('',#8903);
#3266=VERTEX_POINT('',#8904);
#3267=VERTEX_POINT('',#8906);
#3268=VERTEX_POINT('',#8908);
#3269=VERTEX_POINT('',#8910);
#3270=VERTEX_POINT('',#8912);
#3271=VERTEX_POINT('',#8916);
#3272=VERTEX_POINT('',#8917);
#3273=VERTEX_POINT('',#8919);
#3274=VERTEX_POINT('',#8921);
#3275=VERTEX_POINT('',#8923);
#3276=VERTEX_POINT('',#8927);
#3277=VERTEX_POINT('',#8928);
#3278=VERTEX_POINT('',#8930);
#3279=VERTEX_POINT('',#8932);
#3280=VERTEX_POINT('',#8936);
#3281=VERTEX_POINT('',#8937);
#3282=VERTEX_POINT('',#8939);
#3283=VERTEX_POINT('',#8941);
#3284=VERTEX_POINT('',#8943);
#3285=VERTEX_POINT('',#8947);
#3286=VERTEX_POINT('',#8948);
#3287=VERTEX_POINT('',#8950);
#3288=VERTEX_POINT('',#8952);
#3289=VERTEX_POINT('',#8956);
#3290=VERTEX_POINT('',#8957);
#3291=VERTEX_POINT('',#8959);
#3292=VERTEX_POINT('',#8961);
#3293=VERTEX_POINT('',#8963);
#3294=VERTEX_POINT('',#8968);
#3295=VERTEX_POINT('',#8970);
#3296=VERTEX_POINT('',#8998);
#3297=VERTEX_POINT('',#9000);
#3298=VERTEX_POINT('',#9008);
#3299=VERTEX_POINT('',#9010);
#3300=VERTEX_POINT('',#9020);
#3301=VERTEX_POINT('',#9021);
#3302=VERTEX_POINT('',#9023);
#3303=VERTEX_POINT('',#9025);
#3304=VERTEX_POINT('',#9032);
#3305=VERTEX_POINT('',#9034);
#3306=VERTEX_POINT('',#9037);
#3307=VERTEX_POINT('',#9039);
#3308=VERTEX_POINT('',#9043);
#3309=VERTEX_POINT('',#9045);
#3310=VERTEX_POINT('',#9049);
#3311=VERTEX_POINT('',#9051);
#3312=VERTEX_POINT('',#9053);
#3313=VERTEX_POINT('',#9057);
#3314=VERTEX_POINT('',#9064);
#3315=VERTEX_POINT('',#9066);
#3316=VERTEX_POINT('',#9068);
#3317=VERTEX_POINT('',#9070);
#3318=VERTEX_POINT('',#9074);
#3319=VERTEX_POINT('',#9076);
#3320=VERTEX_POINT('',#9083);
#3321=VERTEX_POINT('',#9092);
#3322=VERTEX_POINT('',#9094);
#3323=VERTEX_POINT('',#9100);
#3324=VERTEX_POINT('',#9102);
#3325=VERTEX_POINT('',#9104);
#3326=VERTEX_POINT('',#9105);
#3327=VERTEX_POINT('',#9107);
#3328=VERTEX_POINT('',#9109);
#3329=VERTEX_POINT('',#9112);
#3330=VERTEX_POINT('',#9115);
#3331=VERTEX_POINT('',#9116);
#3332=VERTEX_POINT('',#9118);
#3333=VERTEX_POINT('',#9120);
#3334=VERTEX_POINT('',#9123);
#3335=VERTEX_POINT('',#9135);
#3336=VERTEX_POINT('',#9137);
#3337=VERTEX_POINT('',#9141);
#3338=VERTEX_POINT('',#9145);
#3339=VERTEX_POINT('',#9147);
#3340=VERTEX_POINT('',#9151);
#3341=VERTEX_POINT('',#9156);
#3342=VERTEX_POINT('',#9157);
#3343=VERTEX_POINT('',#9159);
#3344=VERTEX_POINT('',#9161);
#3345=VERTEX_POINT('',#9165);
#3346=VERTEX_POINT('',#9167);
#3347=VERTEX_POINT('',#9171);
#3348=VERTEX_POINT('',#9173);
#3349=VERTEX_POINT('',#9177);
#3350=VERTEX_POINT('',#9179);
#3351=VERTEX_POINT('',#9185);
#3352=VERTEX_POINT('',#9187);
#3353=VERTEX_POINT('',#9190);
#3354=VERTEX_POINT('',#9192);
#3355=VERTEX_POINT('',#9195);
#3356=VERTEX_POINT('',#9197);
#3357=VERTEX_POINT('',#9200);
#3358=VERTEX_POINT('',#9202);
#3359=VERTEX_POINT('',#9205);
#3360=VERTEX_POINT('',#9208);
#3361=VERTEX_POINT('',#9213);
#3362=VERTEX_POINT('',#9215);
#3363=VERTEX_POINT('',#9217);
#3364=VERTEX_POINT('',#9219);
#3365=VERTEX_POINT('',#9222);
#3366=VERTEX_POINT('',#9224);
#3367=VERTEX_POINT('',#9226);
#3368=VERTEX_POINT('',#9228);
#3369=VERTEX_POINT('',#9236);
#3370=VERTEX_POINT('',#9238);
#3371=VERTEX_POINT('',#9241);
#3372=VERTEX_POINT('',#9243);
#3373=VERTEX_POINT('',#9246);
#3374=VERTEX_POINT('',#9247);
#3375=VERTEX_POINT('',#9249);
#3376=VERTEX_POINT('',#9251);
#3377=VERTEX_POINT('',#9253);
#3378=VERTEX_POINT('',#9255);
#3379=VERTEX_POINT('',#9257);
#3380=VERTEX_POINT('',#9259);
#3381=VERTEX_POINT('',#9261);
#3382=VERTEX_POINT('',#9263);
#3383=VERTEX_POINT('',#9265);
#3384=VERTEX_POINT('',#9267);
#3385=VERTEX_POINT('',#9269);
#3386=VERTEX_POINT('',#9271);
#3387=VERTEX_POINT('',#9273);
#3388=VERTEX_POINT('',#9275);
#3389=VERTEX_POINT('',#9277);
#3390=VERTEX_POINT('',#9279);
#3391=VERTEX_POINT('',#9281);
#3392=VERTEX_POINT('',#9283);
#3393=VERTEX_POINT('',#9285);
#3394=VERTEX_POINT('',#9287);
#3395=VERTEX_POINT('',#9289);
#3396=VERTEX_POINT('',#9291);
#3397=VERTEX_POINT('',#9293);
#3398=VERTEX_POINT('',#9295);
#3399=VERTEX_POINT('',#9297);
#3400=VERTEX_POINT('',#9299);
#3401=VERTEX_POINT('',#9301);
#3402=VERTEX_POINT('',#9303);
#3403=VERTEX_POINT('',#9305);
#3404=VERTEX_POINT('',#9307);
#3405=VERTEX_POINT('',#9309);
#3406=VERTEX_POINT('',#9311);
#3407=VERTEX_POINT('',#9313);
#3408=VERTEX_POINT('',#9315);
#3409=VERTEX_POINT('',#9317);
#3410=VERTEX_POINT('',#9319);
#3411=VERTEX_POINT('',#9321);
#3412=VERTEX_POINT('',#9323);
#3413=VERTEX_POINT('',#9325);
#3414=VERTEX_POINT('',#9327);
#3415=VERTEX_POINT('',#9329);
#3416=VERTEX_POINT('',#9331);
#3417=VERTEX_POINT('',#9333);
#3418=VERTEX_POINT('',#9335);
#3419=VERTEX_POINT('',#9337);
#3420=VERTEX_POINT('',#9339);
#3421=VERTEX_POINT('',#9341);
#3422=VERTEX_POINT('',#9343);
#3423=VERTEX_POINT('',#9345);
#3424=VERTEX_POINT('',#9347);
#3425=VERTEX_POINT('',#9349);
#3426=VERTEX_POINT('',#9351);
#3427=VERTEX_POINT('',#9353);
#3428=VERTEX_POINT('',#9355);
#3429=VERTEX_POINT('',#9357);
#3430=VERTEX_POINT('',#9359);
#3431=VERTEX_POINT('',#9361);
#3432=VERTEX_POINT('',#9363);
#3433=VERTEX_POINT('',#9365);
#3434=VERTEX_POINT('',#9367);
#3435=VERTEX_POINT('',#9369);
#3436=VERTEX_POINT('',#9371);
#3437=VERTEX_POINT('',#9373);
#3438=VERTEX_POINT('',#9375);
#3439=VERTEX_POINT('',#9377);
#3440=VERTEX_POINT('',#9379);
#3441=VERTEX_POINT('',#9381);
#3442=VERTEX_POINT('',#9383);
#3443=VERTEX_POINT('',#9385);
#3444=VERTEX_POINT('',#9387);
#3445=VERTEX_POINT('',#9389);
#3446=VERTEX_POINT('',#9391);
#3447=VERTEX_POINT('',#9393);
#3448=VERTEX_POINT('',#9395);
#3449=VERTEX_POINT('',#9397);
#3450=VERTEX_POINT('',#9399);
#3451=VERTEX_POINT('',#9401);
#3452=VERTEX_POINT('',#9403);
#3453=VERTEX_POINT('',#9405);
#3454=VERTEX_POINT('',#9407);
#3455=VERTEX_POINT('',#9409);
#3456=VERTEX_POINT('',#9411);
#3457=VERTEX_POINT('',#9413);
#3458=VERTEX_POINT('',#9415);
#3459=VERTEX_POINT('',#9417);
#3460=VERTEX_POINT('',#9419);
#3461=VERTEX_POINT('',#9423);
#3462=VERTEX_POINT('',#9425);
#3463=VERTEX_POINT('',#9429);
#3464=VERTEX_POINT('',#9431);
#3465=VERTEX_POINT('',#9435);
#3466=VERTEX_POINT('',#9437);
#3467=VERTEX_POINT('',#9441);
#3468=VERTEX_POINT('',#9443);
#3469=VERTEX_POINT('',#9447);
#3470=VERTEX_POINT('',#9449);
#3471=VERTEX_POINT('',#9453);
#3472=VERTEX_POINT('',#9455);
#3473=VERTEX_POINT('',#9459);
#3474=VERTEX_POINT('',#9461);
#3475=VERTEX_POINT('',#9465);
#3476=VERTEX_POINT('',#9467);
#3477=VERTEX_POINT('',#9471);
#3478=VERTEX_POINT('',#9473);
#3479=VERTEX_POINT('',#9477);
#3480=VERTEX_POINT('',#9479);
#3481=VERTEX_POINT('',#9483);
#3482=VERTEX_POINT('',#9485);
#3483=VERTEX_POINT('',#9489);
#3484=VERTEX_POINT('',#9491);
#3485=VERTEX_POINT('',#9495);
#3486=VERTEX_POINT('',#9497);
#3487=VERTEX_POINT('',#9501);
#3488=VERTEX_POINT('',#9503);
#3489=VERTEX_POINT('',#9507);
#3490=VERTEX_POINT('',#9509);
#3491=VERTEX_POINT('',#9513);
#3492=VERTEX_POINT('',#9515);
#3493=VERTEX_POINT('',#9519);
#3494=VERTEX_POINT('',#9521);
#3495=VERTEX_POINT('',#9525);
#3496=VERTEX_POINT('',#9527);
#3497=VERTEX_POINT('',#9531);
#3498=VERTEX_POINT('',#9533);
#3499=VERTEX_POINT('',#9537);
#3500=VERTEX_POINT('',#9539);
#3501=VERTEX_POINT('',#9543);
#3502=VERTEX_POINT('',#9545);
#3503=VERTEX_POINT('',#9549);
#3504=VERTEX_POINT('',#9551);
#3505=VERTEX_POINT('',#9553);
#3506=VERTEX_POINT('',#9556);
#3507=VERTEX_POINT('',#9558);
#3508=VERTEX_POINT('',#9561);
#3509=VERTEX_POINT('',#9563);
#3510=VERTEX_POINT('',#9566);
#3511=VERTEX_POINT('',#9568);
#3512=VERTEX_POINT('',#9571);
#3513=VERTEX_POINT('',#9573);
#3514=VERTEX_POINT('',#9575);
#3515=VERTEX_POINT('',#9577);
#3516=VERTEX_POINT('',#9579);
#3517=VERTEX_POINT('',#9581);
#3518=VERTEX_POINT('',#9584);
#3519=VERTEX_POINT('',#9586);
#3520=VERTEX_POINT('',#9589);
#3521=VERTEX_POINT('',#9591);
#3522=VERTEX_POINT('',#9594);
#3523=VERTEX_POINT('',#9596);
#3524=VERTEX_POINT('',#9599);
#3525=VERTEX_POINT('',#9601);
#3526=VERTEX_POINT('',#9604);
#3527=VERTEX_POINT('',#9606);
#3528=VERTEX_POINT('',#9609);
#3529=VERTEX_POINT('',#9611);
#3530=VERTEX_POINT('',#9614);
#3531=VERTEX_POINT('',#9616);
#3532=VERTEX_POINT('',#9619);
#3533=VERTEX_POINT('',#9621);
#3534=VERTEX_POINT('',#9624);
#3535=VERTEX_POINT('',#9626);
#3536=VERTEX_POINT('',#9629);
#3537=VERTEX_POINT('',#9631);
#3538=VERTEX_POINT('',#9634);
#3539=VERTEX_POINT('',#9636);
#3540=VERTEX_POINT('',#9639);
#3541=VERTEX_POINT('',#9641);
#3542=VERTEX_POINT('',#9644);
#3543=VERTEX_POINT('',#9646);
#3544=VERTEX_POINT('',#9649);
#3545=VERTEX_POINT('',#9651);
#3546=VERTEX_POINT('',#9654);
#3547=VERTEX_POINT('',#9656);
#3548=VERTEX_POINT('',#9659);
#3549=VERTEX_POINT('',#9776);
#3550=VERTEX_POINT('',#9778);
#3551=VERTEX_POINT('',#9781);
#3552=VERTEX_POINT('',#9786);
#3553=VERTEX_POINT('',#9788);
#3554=VERTEX_POINT('',#9791);
#3555=VERTEX_POINT('',#9797);
#3556=VERTEX_POINT('',#9798);
#3557=VERTEX_POINT('',#9800);
#3558=VERTEX_POINT('',#9802);
#3559=VERTEX_POINT('',#9806);
#3560=VERTEX_POINT('',#9808);
#3561=VERTEX_POINT('',#9812);
#3562=VERTEX_POINT('',#9814);
#3563=VERTEX_POINT('',#9821);
#3564=VERTEX_POINT('',#9824);
#3565=VERTEX_POINT('',#9829);
#3566=VERTEX_POINT('',#9830);
#3567=VERTEX_POINT('',#9832);
#3568=VERTEX_POINT('',#9840);
#3569=VERTEX_POINT('',#9844);
#3570=VERTEX_POINT('',#9846);
#3571=VERTEX_POINT('',#9850);
#3572=VERTEX_POINT('',#9852);
#3573=VERTEX_POINT('',#9871);
#3574=VERTEX_POINT('',#9872);
#3575=VERTEX_POINT('',#9874);
#3576=VERTEX_POINT('',#9882);
#3577=VERTEX_POINT('',#9886);
#3578=VERTEX_POINT('',#9887);
#3579=VERTEX_POINT('',#9889);
#3580=VERTEX_POINT('',#9891);
#3581=VERTEX_POINT('',#9905);
#3582=VERTEX_POINT('',#9907);
#3583=VERTEX_POINT('',#9908);
#3584=VERTEX_POINT('',#9910);
#3585=VERTEX_POINT('',#9912);
#3586=VERTEX_POINT('',#9915);
#3587=VERTEX_POINT('',#9918);
#3588=VERTEX_POINT('',#9919);
#3589=VERTEX_POINT('',#9921);
#3590=VERTEX_POINT('',#9923);
#3591=VERTEX_POINT('',#9926);
#3592=VERTEX_POINT('',#9928);
#3593=VERTEX_POINT('',#9942);
#3594=VERTEX_POINT('',#9944);
#3595=VERTEX_POINT('',#9947);
#3596=VERTEX_POINT('',#9950);
#3597=VERTEX_POINT('',#9953);
#3598=VERTEX_POINT('',#9956);
#3599=VERTEX_POINT('',#9959);
#3600=VERTEX_POINT('',#9961);
#3601=VERTEX_POINT('',#9964);
#3602=VERTEX_POINT('',#9966);
#3603=VERTEX_POINT('',#9969);
#3604=VERTEX_POINT('',#9971);
#3605=VERTEX_POINT('',#9975);
#3606=VERTEX_POINT('',#9979);
#3607=VERTEX_POINT('',#9982);
#3608=VERTEX_POINT('',#9985);
#3609=VERTEX_POINT('',#9991);
#3610=VERTEX_POINT('',#9992);
#3611=VERTEX_POINT('',#9994);
#3612=VERTEX_POINT('',#9996);
#3613=VERTEX_POINT('',#9998);
#3614=VERTEX_POINT('',#10000);
#3615=VERTEX_POINT('',#10002);
#3616=VERTEX_POINT('',#10004);
#3617=VERTEX_POINT('',#10006);
#3618=VERTEX_POINT('',#10008);
#3619=VERTEX_POINT('',#10010);
#3620=VERTEX_POINT('',#10013);
#3621=VERTEX_POINT('',#10016);
#3622=VERTEX_POINT('',#10017);
#3623=VERTEX_POINT('',#10019);
#3624=VERTEX_POINT('',#10021);
#3625=VERTEX_POINT('',#10023);
#3626=VERTEX_POINT('',#10025);
#3627=VERTEX_POINT('',#10027);
#3628=VERTEX_POINT('',#10029);
#3629=VERTEX_POINT('',#10031);
#3630=VERTEX_POINT('',#10033);
#3631=VERTEX_POINT('',#10035);
#3632=VERTEX_POINT('',#10038);
#3633=VERTEX_POINT('',#10065);
#3634=VERTEX_POINT('',#10066);
#3635=VERTEX_POINT('',#10070);
#3636=VERTEX_POINT('',#10071);
#3637=VERTEX_POINT('',#10076);
#3638=VERTEX_POINT('',#10078);
#3639=VERTEX_POINT('',#10085);
#3640=VERTEX_POINT('',#10087);
#3641=VERTEX_POINT('',#10090);
#3642=VERTEX_POINT('',#10095);
#3643=VERTEX_POINT('',#10096);
#3644=VERTEX_POINT('',#10101);
#3645=VERTEX_POINT('',#10103);
#3646=VERTEX_POINT('',#10112);
#3647=VERTEX_POINT('',#10114);
#3648=VERTEX_POINT('',#10120);
#3649=VERTEX_POINT('',#10123);
#3650=CIRCLE('',#5706,0.06);
#3651=CIRCLE('',#5707,0.06);
#3652=CIRCLE('',#5709,0.061);
#3653=CIRCLE('',#5710,0.061);
#3654=CIRCLE('',#5712,0.0635);
#3655=CIRCLE('',#5714,0.0015);
#3656=CIRCLE('',#5715,0.0015);
#3657=CIRCLE('',#5716,0.0015);
#3658=CIRCLE('',#5717,0.0015);
#3659=CIRCLE('',#5719,0.0635);
#3660=CIRCLE('',#5722,0.0015);
#3661=CIRCLE('',#5723,0.0015);
#3662=CIRCLE('',#5724,0.0015);
#3663=CIRCLE('',#5725,0.0015);
#3664=CIRCLE('',#5733,0.0020008872882516);
#3665=CIRCLE('',#5735,0.00210050675806077);
#3666=CIRCLE('',#5736,0.0020008872882516);
#3667=CIRCLE('',#5738,0.00125);
#3668=CIRCLE('',#5739,0.00125);
#3669=CIRCLE('',#5741,0.00100643035625);
#3670=CIRCLE('',#5744,0.00210050675806077);
#3671=CIRCLE('',#5745,0.00215376247012148);
#3672=CIRCLE('',#5746,0.00215376247012148);
#3673=CIRCLE('',#5747,0.00225);
#3674=CIRCLE('',#5749,0.00135);
#3675=CIRCLE('',#5759,0.0125);
#3676=CIRCLE('',#5760,0.0125);
#3677=CIRCLE('',#5762,0.0125);
#3678=CIRCLE('',#5763,0.0125);
#3679=CIRCLE('',#5765,0.0015);
#3680=CIRCLE('',#5766,0.0015);
#3681=CIRCLE('',#5768,0.0015);
#3682=CIRCLE('',#5769,0.0015);
#3683=CIRCLE('',#5770,0.0048);
#3684=CIRCLE('',#5771,0.011374);
#3685=CIRCLE('',#5772,0.0048);
#3686=CIRCLE('',#5773,0.0125);
#3687=CIRCLE('',#5774,0.0048);
#3688=CIRCLE('',#5775,0.011374);
#3689=CIRCLE('',#5776,0.0048);
#3690=CIRCLE('',#5777,0.0125);
#3691=CIRCLE('',#5778,0.0048);
#3692=CIRCLE('',#5779,0.011374);
#3693=CIRCLE('',#5780,0.0048);
#3694=CIRCLE('',#5781,0.0125);
#3695=CIRCLE('',#5782,0.0048);
#3696=CIRCLE('',#5783,0.011374);
#3697=CIRCLE('',#5784,0.0048);
#3698=CIRCLE('',#5785,0.0125);
#3699=CIRCLE('',#5786,0.0048);
#3700=CIRCLE('',#5787,0.011374);
#3701=CIRCLE('',#5788,0.0048);
#3702=CIRCLE('',#5789,0.0125);
#3703=CIRCLE('',#5790,0.0048);
#3704=CIRCLE('',#5791,0.011374);
#3705=CIRCLE('',#5792,0.0048);
#3706=CIRCLE('',#5793,0.0125);
#3707=CIRCLE('',#5794,0.0048);
#3708=CIRCLE('',#5795,0.011374);
#3709=CIRCLE('',#5796,0.0048);
#3710=CIRCLE('',#5797,0.0125);
#3711=CIRCLE('',#5798,0.0048);
#3712=CIRCLE('',#5799,0.011374);
#3713=CIRCLE('',#5800,0.0048);
#3714=CIRCLE('',#5801,0.0125);
#3715=CIRCLE('',#5802,0.0048);
#3716=CIRCLE('',#5803,0.011374);
#3717=CIRCLE('',#5804,0.0048);
#3718=CIRCLE('',#5805,0.0125);
#3719=CIRCLE('',#5806,0.0048);
#3720=CIRCLE('',#5807,0.011374);
#3721=CIRCLE('',#5808,0.0048);
#3722=CIRCLE('',#5809,0.0125);
#3723=CIRCLE('',#5810,0.0048);
#3724=CIRCLE('',#5811,0.011374);
#3725=CIRCLE('',#5812,0.0048);
#3726=CIRCLE('',#5813,0.015);
#3727=CIRCLE('',#5814,0.00499999999999989);
#3728=CIRCLE('',#5815,0.005);
#3729=CIRCLE('',#5816,0.0354217830972575);
#3730=CIRCLE('',#5818,0.0048);
#3731=CIRCLE('',#5819,0.0354217830972575);
#3732=CIRCLE('',#5820,0.005);
#3733=CIRCLE('',#5821,0.00499999999999989);
#3734=CIRCLE('',#5822,0.015);
#3735=CIRCLE('',#5823,0.0048);
#3736=CIRCLE('',#5824,0.011374);
#3737=CIRCLE('',#5825,0.0048);
#3738=CIRCLE('',#5826,0.0125);
#3739=CIRCLE('',#5827,0.0048);
#3740=CIRCLE('',#5828,0.011374);
#3741=CIRCLE('',#5829,0.0048);
#3742=CIRCLE('',#5830,0.0125);
#3743=CIRCLE('',#5831,0.0048);
#3744=CIRCLE('',#5832,0.011374);
#3745=CIRCLE('',#5833,0.0048);
#3746=CIRCLE('',#5834,0.0125);
#3747=CIRCLE('',#5835,0.0048);
#3748=CIRCLE('',#5836,0.011374);
#3749=CIRCLE('',#5837,0.0048);
#3750=CIRCLE('',#5838,0.0125);
#3751=CIRCLE('',#5839,0.0048);
#3752=CIRCLE('',#5840,0.011374);
#3753=CIRCLE('',#5841,0.0048);
#3754=CIRCLE('',#5842,0.0125);
#3755=CIRCLE('',#5843,0.0048);
#3756=CIRCLE('',#5844,0.011374);
#3757=CIRCLE('',#5845,0.0048);
#3758=CIRCLE('',#5846,0.0125);
#3759=CIRCLE('',#5847,0.0048);
#3760=CIRCLE('',#5848,0.011374);
#3761=CIRCLE('',#5849,0.0048);
#3762=CIRCLE('',#5850,0.0125);
#3763=CIRCLE('',#5851,0.0048);
#3764=CIRCLE('',#5852,0.011374);
#3765=CIRCLE('',#5853,0.0048);
#3766=CIRCLE('',#5854,0.0125);
#3767=CIRCLE('',#5855,0.0048);
#3768=CIRCLE('',#5856,0.011374);
#3769=CIRCLE('',#5857,0.0048);
#3770=CIRCLE('',#5858,0.0125);
#3771=CIRCLE('',#5859,0.0048);
#3772=CIRCLE('',#5860,0.011374);
#3773=CIRCLE('',#5861,0.0048);
#3774=CIRCLE('',#5862,0.0125);
#3775=CIRCLE('',#5863,0.0048);
#3776=CIRCLE('',#5864,0.011374);
#3777=CIRCLE('',#5865,0.0015);
#3778=CIRCLE('',#5866,0.0015);
#3779=CIRCLE('',#5926,0.002);
#3780=CIRCLE('',#5927,0.002);
#3781=CIRCLE('',#5934,0.002);
#3782=CIRCLE('',#5935,0.002);
#3783=CIRCLE('',#5937,0.002);
#3784=CIRCLE('',#5938,0.002);
#3785=CIRCLE('',#5940,0.002);
#3786=CIRCLE('',#5941,0.002);
#3787=CIRCLE('',#5943,0.002);
#3788=CIRCLE('',#5944,0.002);
#3789=CIRCLE('',#5946,0.002);
#3790=CIRCLE('',#5947,0.002);
#3791=CIRCLE('',#5949,0.002);
#3792=CIRCLE('',#5950,0.002);
#3793=CIRCLE('',#5952,0.002);
#3794=CIRCLE('',#5953,0.002);
#3795=CIRCLE('',#5955,0.002);
#3796=CIRCLE('',#5956,0.002);
#3797=CIRCLE('',#5958,0.002);
#3798=CIRCLE('',#5959,0.002);
#3799=CIRCLE('',#5961,0.006);
#3800=CIRCLE('',#5963,0.006);
#3801=CIRCLE('',#5965,0.006);
#3802=CIRCLE('',#5967,0.0015);
#3803=CIRCLE('',#5969,0.006);
#3804=CIRCLE('',#5972,0.004);
#3805=CIRCLE('',#5973,0.004);
#3806=CIRCLE('',#5975,0.0015);
#3807=CIRCLE('',#5976,0.0025);
#3808=CIRCLE('',#5979,0.002);
#3809=CIRCLE('',#5981,0.0015);
#3810=CIRCLE('',#5983,0.002);
#3811=CIRCLE('',#5986,0.0015);
#3812=CIRCLE('',#5987,0.0015);
#3813=CIRCLE('',#5989,0.0015);
#3814=CIRCLE('',#5991,0.0015);
#3815=CIRCLE('',#5993,0.0015);
#3816=CIRCLE('',#5999,0.00500637669063053);
#3817=CIRCLE('',#6000,0.00500637669063053);
#3818=CIRCLE('',#6005,0.002);
#3819=CIRCLE('',#6006,0.002);
#3820=CIRCLE('',#6007,0.003);
#3821=CIRCLE('',#6008,0.003);
#3822=CIRCLE('',#6009,0.0025);
#3823=CIRCLE('',#6011,0.003);
#3824=CIRCLE('',#6012,0.003);
#3825=CIRCLE('',#6013,0.0025);
#3826=CIRCLE('',#6020,0.002);
#3827=CIRCLE('',#6021,0.0015);
#3828=CIRCLE('',#6024,0.0015);
#3829=CIRCLE('',#6027,0.002);
#3830=CIRCLE('',#6028,0.0015);
#3831=CIRCLE('',#6031,0.0015);
#3832=CIRCLE('',#6038,0.0015);
#3833=CIRCLE('',#6039,0.0015);
#3834=CIRCLE('',#6042,0.0015);
#3835=CIRCLE('',#6043,0.0015);
#3836=CIRCLE('',#6045,0.0015);
#3837=CIRCLE('',#6046,0.0015);
#3838=CIRCLE('',#6048,0.0015);
#3839=CIRCLE('',#6049,0.0015);
#3840=CIRCLE('',#6051,0.0015);
#3841=CIRCLE('',#6052,0.0015);
#3842=CIRCLE('',#6054,0.0015);
#3843=CIRCLE('',#6056,0.0015);
#3844=CIRCLE('',#6060,0.00250000000000006);
#3845=CIRCLE('',#6061,0.0016601861613766);
#3846=CIRCLE('',#6062,0.00145132271222225);
#3847=CIRCLE('',#6063,0.059);
#3848=CIRCLE('',#6065,0.00250000000000006);
#3849=CIRCLE('',#6066,0.0016601861613766);
#3850=CIRCLE('',#6067,0.00145132271222225);
#3851=CIRCLE('',#6068,0.059);
#3852=CIRCLE('',#6075,0.0015);
#3853=CIRCLE('',#6076,0.0015);
#3854=CIRCLE('',#6078,0.0025);
#3855=CIRCLE('',#6079,0.0025);
#3856=CIRCLE('',#6081,0.0022);
#3857=CIRCLE('',#6082,0.004874);
#3858=CIRCLE('',#6083,0.0022);
#3859=CIRCLE('',#6084,0.006);
#3860=CIRCLE('',#6085,0.0022);
#3861=CIRCLE('',#6086,0.004874);
#3862=CIRCLE('',#6087,0.0022);
#3863=CIRCLE('',#6088,0.006);
#3864=CIRCLE('',#6089,0.0022);
#3865=CIRCLE('',#6090,0.004874);
#3866=CIRCLE('',#6091,0.0022);
#3867=CIRCLE('',#6092,0.006);
#3868=CIRCLE('',#6093,0.0022);
#3869=CIRCLE('',#6094,0.004874);
#3870=CIRCLE('',#6095,0.0022);
#3871=CIRCLE('',#6096,0.006);
#3872=CIRCLE('',#6097,0.0022);
#3873=CIRCLE('',#6098,0.004874);
#3874=CIRCLE('',#6099,0.0022);
#3875=CIRCLE('',#6100,0.006);
#3876=CIRCLE('',#6101,0.0022);
#3877=CIRCLE('',#6102,0.004874);
#3878=CIRCLE('',#6103,0.0022);
#3879=CIRCLE('',#6104,0.006);
#3880=CIRCLE('',#6105,0.0022);
#3881=CIRCLE('',#6106,0.004874);
#3882=CIRCLE('',#6107,0.0022);
#3883=CIRCLE('',#6108,0.006);
#3884=CIRCLE('',#6109,0.0022);
#3885=CIRCLE('',#6110,0.004874);
#3886=CIRCLE('',#6111,0.0022);
#3887=CIRCLE('',#6112,0.006);
#3888=CIRCLE('',#6113,0.0022);
#3889=CIRCLE('',#6114,0.004874);
#3890=CIRCLE('',#6115,0.0022);
#3891=CIRCLE('',#6116,0.006);
#3892=CIRCLE('',#6117,0.0022);
#3893=CIRCLE('',#6118,0.004874);
#3894=CIRCLE('',#6119,0.0022);
#3895=CIRCLE('',#6120,0.006);
#3896=CIRCLE('',#6121,0.0022);
#3897=CIRCLE('',#6122,0.004874);
#3898=CIRCLE('',#6123,0.0022);
#3899=CIRCLE('',#6124,0.006);
#3900=CIRCLE('',#6125,0.0022);
#3901=CIRCLE('',#6126,0.004874);
#3902=CIRCLE('',#6127,0.0022);
#3903=CIRCLE('',#6128,0.006);
#3904=CIRCLE('',#6129,0.0022);
#3905=CIRCLE('',#6130,0.004874);
#3906=CIRCLE('',#6131,0.0022);
#3907=CIRCLE('',#6132,0.006);
#3908=CIRCLE('',#6133,0.0022);
#3909=CIRCLE('',#6134,0.004874);
#3910=CIRCLE('',#6135,0.0022);
#3911=CIRCLE('',#6136,0.006);
#3912=CIRCLE('',#6137,0.0022);
#3913=CIRCLE('',#6138,0.004874);
#3914=CIRCLE('',#6139,0.0022);
#3915=CIRCLE('',#6140,0.006);
#3916=CIRCLE('',#6141,0.0022);
#3917=CIRCLE('',#6142,0.004874);
#3918=CIRCLE('',#6143,0.0022);
#3919=CIRCLE('',#6144,0.006);
#3920=CIRCLE('',#6145,0.0022);
#3921=CIRCLE('',#6146,0.004874);
#3922=CIRCLE('',#6147,0.0022);
#3923=CIRCLE('',#6148,0.006);
#3924=CIRCLE('',#6149,0.0022);
#3925=CIRCLE('',#6150,0.004874);
#3926=CIRCLE('',#6151,0.0022);
#3927=CIRCLE('',#6152,0.006);
#3928=CIRCLE('',#6153,0.0022);
#3929=CIRCLE('',#6154,0.004874);
#3930=CIRCLE('',#6155,0.0022);
#3931=CIRCLE('',#6156,0.006);
#3932=CIRCLE('',#6157,0.0022);
#3933=CIRCLE('',#6158,0.004874);
#3934=CIRCLE('',#6159,0.0022);
#3935=CIRCLE('',#6160,0.006);
#3936=CIRCLE('',#6161,0.0022);
#3937=CIRCLE('',#6162,0.004874);
#3938=CIRCLE('',#6163,0.0022);
#3939=CIRCLE('',#6164,0.006);
#3940=CIRCLE('',#6165,0.0022);
#3941=CIRCLE('',#6166,0.004874);
#3942=CIRCLE('',#6167,0.0022);
#3943=CIRCLE('',#6168,0.006);
#3944=CIRCLE('',#6170,0.006);
#3945=CIRCLE('',#6172,0.006);
#3946=CIRCLE('',#6174,0.006);
#3947=CIRCLE('',#6176,0.006);
#3948=CIRCLE('',#6178,0.006);
#3949=CIRCLE('',#6180,0.006);
#3950=CIRCLE('',#6182,0.006);
#3951=CIRCLE('',#6184,0.006);
#3952=CIRCLE('',#6186,0.006);
#3953=CIRCLE('',#6188,0.006);
#3954=CIRCLE('',#6190,0.006);
#3955=CIRCLE('',#6192,0.006);
#3956=CIRCLE('',#6194,0.006);
#3957=CIRCLE('',#6196,0.006);
#3958=CIRCLE('',#6198,0.006);
#3959=CIRCLE('',#6200,0.006);
#3960=CIRCLE('',#6202,0.006);
#3961=CIRCLE('',#6204,0.006);
#3962=CIRCLE('',#6206,0.006);
#3963=CIRCLE('',#6208,0.006);
#3964=CIRCLE('',#6210,0.006);
#3965=CIRCLE('',#6212,0.0022);
#3966=CIRCLE('',#6213,0.0022);
#3967=CIRCLE('',#6214,0.004874);
#3968=CIRCLE('',#6215,0.0022);
#3969=CIRCLE('',#6216,0.0022);
#3970=CIRCLE('',#6217,0.004874);
#3971=CIRCLE('',#6218,0.0022);
#3972=CIRCLE('',#6219,0.0022);
#3973=CIRCLE('',#6220,0.004874);
#3974=CIRCLE('',#6221,0.0022);
#3975=CIRCLE('',#6222,0.0022);
#3976=CIRCLE('',#6223,0.004874);
#3977=CIRCLE('',#6224,0.0022);
#3978=CIRCLE('',#6225,0.0022);
#3979=CIRCLE('',#6226,0.004874);
#3980=CIRCLE('',#6227,0.0022);
#3981=CIRCLE('',#6228,0.006);
#3982=CIRCLE('',#6229,0.0022);
#3983=CIRCLE('',#6230,0.004874);
#3984=CIRCLE('',#6231,0.0022);
#3985=CIRCLE('',#6232,0.0022);
#3986=CIRCLE('',#6233,0.004874);
#3987=CIRCLE('',#6234,0.0022);
#3988=CIRCLE('',#6235,0.0022);
#3989=CIRCLE('',#6236,0.004874);
#3990=CIRCLE('',#6237,0.0022);
#3991=CIRCLE('',#6238,0.0022);
#3992=CIRCLE('',#6239,0.004874);
#3993=CIRCLE('',#6240,0.0022);
#3994=CIRCLE('',#6241,0.0022);
#3995=CIRCLE('',#6242,0.004874);
#3996=CIRCLE('',#6243,0.0022);
#3997=CIRCLE('',#6244,0.0022);
#3998=CIRCLE('',#6245,0.004874);
#3999=CIRCLE('',#6246,0.0022);
#4000=CIRCLE('',#6247,0.0022);
#4001=CIRCLE('',#6248,0.004874);
#4002=CIRCLE('',#6249,0.0022);
#4003=CIRCLE('',#6250,0.0022);
#4004=CIRCLE('',#6251,0.004874);
#4005=CIRCLE('',#6252,0.0022);
#4006=CIRCLE('',#6253,0.0022);
#4007=CIRCLE('',#6254,0.004874);
#4008=CIRCLE('',#6255,0.0022);
#4009=CIRCLE('',#6256,0.0022);
#4010=CIRCLE('',#6257,0.004874);
#4011=CIRCLE('',#6258,0.0022);
#4012=CIRCLE('',#6259,0.0022);
#4013=CIRCLE('',#6260,0.004874);
#4014=CIRCLE('',#6261,0.0022);
#4015=CIRCLE('',#6262,0.0022);
#4016=CIRCLE('',#6263,0.004874);
#4017=CIRCLE('',#6264,0.0022);
#4018=CIRCLE('',#6265,0.0022);
#4019=CIRCLE('',#6266,0.004874);
#4020=CIRCLE('',#6267,0.0022);
#4021=CIRCLE('',#6268,0.0022);
#4022=CIRCLE('',#6269,0.004874);
#4023=CIRCLE('',#6270,0.0022);
#4024=CIRCLE('',#6271,0.0022);
#4025=CIRCLE('',#6272,0.004874);
#4026=CIRCLE('',#6273,0.0022);
#4027=CIRCLE('',#6274,0.0022);
#4028=CIRCLE('',#6275,0.004874);
#4029=CIRCLE('',#6276,0.0022);
#4030=CIRCLE('',#6277,0.0022);
#4031=CIRCLE('',#6278,0.004874);
#4032=CIRCLE('',#6347,0.0025);
#4033=CIRCLE('',#6348,0.00375738138352587);
#4034=CIRCLE('',#6350,0.00375738138352587);
#4035=CIRCLE('',#6354,0.0015);
#4036=CIRCLE('',#6355,0.0015);
#4037=CIRCLE('',#6357,0.0025);
#4038=CIRCLE('',#6362,0.051);
#4039=CIRCLE('',#6363,0.051);
#4040=CIRCLE('',#6365,0.002);
#4041=CIRCLE('',#6366,0.002);
#4042=CIRCLE('',#6368,0.049);
#4043=CIRCLE('',#6369,0.049);
#4044=CIRCLE('',#6372,0.0015);
#4045=CIRCLE('',#6374,0.0015);
#4046=CIRCLE('',#6378,0.0015);
#4047=CIRCLE('',#6379,0.0485);
#4048=CIRCLE('',#6380,0.0515);
#4049=CIRCLE('',#6382,0.0485);
#4050=CIRCLE('',#6384,0.0015);
#4051=CIRCLE('',#6385,0.0515);
#4052=CIRCLE('',#6389,0.0025);
#4053=CIRCLE('',#6390,0.0025);
#4054=CIRCLE('',#6392,0.0525);
#4055=CIRCLE('',#6393,0.0475);
#4056=CIRCLE('',#6395,0.0475);
#4057=CIRCLE('',#6397,0.0525);
#4058=CIRCLE('',#6402,0.0015);
#4059=CIRCLE('',#6403,0.002);
#4060=CIRCLE('',#6404,0.002);
#4061=CIRCLE('',#6405,0.0015);
#4062=CIRCLE('',#6407,0.002);
#4063=CIRCLE('',#6408,0.002);
#4064=CIRCLE('',#6409,0.0015);
#4065=CIRCLE('',#6410,0.0015);
#4066=CIRCLE('',#6419,0.0635);
#4067=CIRCLE('',#6420,0.0635);
#4068=CIRCLE('',#6422,0.06);
#4069=CIRCLE('',#6424,0.06);
#4070=CIRCLE('',#6426,0.0619081467766146);
#4071=CIRCLE('',#6428,0.0636093675261996);
#4072=CIRCLE('',#6430,0.0645);
#4073=CIRCLE('',#6431,0.0645);
#4074=CIRCLE('',#6433,0.0629081467766146);
#4075=CIRCLE('',#6434,0.0644389218390369);
#4076=CIRCLE('',#6436,0.0619081467766146);
#4077=CIRCLE('',#6437,0.0619081467766146);
#4078=CIRCLE('',#6440,0.0637040733883139);
#4079=CIRCLE('',#6443,0.0629081467766146);
#4080=CIRCLE('',#6445,0.0635431988692856);
#4081=CIRCLE('',#6447,0.0645);
#4082=CIRCLE('',#6452,0.000257682665739803);
#4083=CIRCLE('',#6453,0.00755256285496241);
#4084=CIRCLE('',#6454,0.0025);
#4085=CIRCLE('',#6455,0.0025);
#4086=CIRCLE('',#6456,0.00755256285496241);
#4087=CIRCLE('',#6457,0.000257682665739803);
#4088=CIRCLE('',#6458,0.0015);
#4089=CIRCLE('',#6460,0.000257682665739803);
#4090=CIRCLE('',#6461,0.000257682665739803);
#4091=CIRCLE('',#6462,0.00755256285496241);
#4092=CIRCLE('',#6463,0.0025);
#4093=CIRCLE('',#6464,0.0025);
#4094=CIRCLE('',#6465,0.00755256285496241);
#4095=CIRCLE('',#6466,0.0015);
#4096=CIRCLE('',#6481,0.0020008872882516);
#4097=CIRCLE('',#6483,0.00210050675806077);
#4098=CIRCLE('',#6484,0.0020008872882516);
#4099=CIRCLE('',#6486,0.00125);
#4100=CIRCLE('',#6487,0.00125);
#4101=CIRCLE('',#6489,0.00100643035625);
#4102=CIRCLE('',#6492,0.00210050675806077);
#4103=CIRCLE('',#6493,0.00215376247012148);
#4104=CIRCLE('',#6494,0.00215376247012148);
#4105=CIRCLE('',#6495,0.00225);
#4106=CIRCLE('',#6497,0.00135);
#4107=EDGE_LOOP('',(#814));
#4108=EDGE_LOOP('',(#815));
#4109=EDGE_LOOP('',(#816));
#4110=EDGE_LOOP('',(#817));
#4111=EDGE_LOOP('',(#818));
#4112=EDGE_LOOP('',(#819));
#4113=EDGE_LOOP('',(#820));
#4114=EDGE_LOOP('',(#821));
#4115=EDGE_LOOP('',(#822));
#4116=EDGE_LOOP('',(#823));
#4117=EDGE_LOOP('',(#824));
#4118=EDGE_LOOP('',(#825));
#4119=EDGE_LOOP('',(#826));
#4120=EDGE_LOOP('',(#827));
#4121=EDGE_LOOP('',(#828));
#4122=EDGE_LOOP('',(#829));
#4123=EDGE_LOOP('',(#830));
#4124=EDGE_LOOP('',(#831));
#4125=EDGE_LOOP('',(#832));
#4126=EDGE_LOOP('',(#833));
#4127=EDGE_LOOP('',(#834));
#4128=EDGE_LOOP('',(#835));
#4129=EDGE_LOOP('',(#836));
#4130=EDGE_LOOP('',(#837));
#4131=EDGE_LOOP('',(#838));
#4132=EDGE_LOOP('',(#839));
#4133=EDGE_LOOP('',(#840));
#4134=EDGE_LOOP('',(#841));
#4135=EDGE_LOOP('',(#842));
#4136=EDGE_LOOP('',(#843));
#4137=EDGE_LOOP('',(#844));
#4138=EDGE_LOOP('',(#845));
#4139=EDGE_LOOP('',(#846,#847));
#4140=EDGE_LOOP('',(#848,#849,#850,#851));
#4141=EDGE_LOOP('',(#852));
#4142=EDGE_LOOP('',(#853));
#4143=EDGE_LOOP('',(#854));
#4144=EDGE_LOOP('',(#855,#856));
#4145=EDGE_LOOP('',(#857,#858,#859,#860,#861,#862,#863,#864));
#4146=EDGE_LOOP('',(#865));
#4147=EDGE_LOOP('',(#866));
#4148=EDGE_LOOP('',(#867));
#4149=EDGE_LOOP('',(#868));
#4150=EDGE_LOOP('',(#869));
#4151=EDGE_LOOP('',(#870,#871,#872,#873));
#4152=EDGE_LOOP('',(#874,#875,#876,#877));
#4153=EDGE_LOOP('',(#878,#879,#880,#881,#882,#883));
#4154=EDGE_LOOP('',(#884,#885,#886,#887,#888,#889));
#4155=EDGE_LOOP('',(#890));
#4156=EDGE_LOOP('',(#891));
#4157=EDGE_LOOP('',(#892,#893,#894,#895));
#4158=EDGE_LOOP('',(#896,#897,#898,#899));
#4159=EDGE_LOOP('',(#900));
#4160=EDGE_LOOP('',(#901));
#4161=EDGE_LOOP('',(#902));
#4162=EDGE_LOOP('',(#903,#904,#905,#906));
#4163=EDGE_LOOP('',(#907,#908,#909,#910,#911,#912,#913,#914,#915,#916,#917,
#918,#919,#920,#921,#922,#923,#924,#925,#926,#927,#928,#929,#930,#931,#932,
#933,#934,#935,#936,#937,#938,#939,#940,#941,#942,#943,#944,#945,#946,#947,
#948,#949,#950,#951,#952,#953,#954,#955,#956,#957,#958));
#4164=EDGE_LOOP('',(#959));
#4165=EDGE_LOOP('',(#960,#961,#962,#963,#964,#965,#966,#967,#968,#969,#970,
#971,#972,#973,#974,#975,#976,#977,#978,#979,#980,#981,#982,#983,#984,#985,
#986,#987,#988,#989,#990,#991,#992,#993,#994,#995,#996,#997,#998,#999,#1000,
#1001,#1002,#1003,#1004,#1005,#1006,#1007,#1008,#1009,#1010,#1011));
#4166=EDGE_LOOP('',(#1012,#1013,#1014,#1015));
#4167=EDGE_LOOP('',(#1016,#1017,#1018,#1019));
#4168=EDGE_LOOP('',(#1020,#1021,#1022,#1023));
#4169=EDGE_LOOP('',(#1024,#1025,#1026,#1027));
#4170=EDGE_LOOP('',(#1028,#1029,#1030,#1031));
#4171=EDGE_LOOP('',(#1032,#1033,#1034,#1035));
#4172=EDGE_LOOP('',(#1036,#1037,#1038,#1039));
#4173=EDGE_LOOP('',(#1040,#1041,#1042,#1043));
#4174=EDGE_LOOP('',(#1044,#1045,#1046,#1047));
#4175=EDGE_LOOP('',(#1048,#1049,#1050,#1051));
#4176=EDGE_LOOP('',(#1052,#1053,#1054,#1055));
#4177=EDGE_LOOP('',(#1056,#1057,#1058,#1059));
#4178=EDGE_LOOP('',(#1060,#1061,#1062,#1063));
#4179=EDGE_LOOP('',(#1064,#1065,#1066,#1067));
#4180=EDGE_LOOP('',(#1068,#1069,#1070,#1071));
#4181=EDGE_LOOP('',(#1072,#1073,#1074,#1075));
#4182=EDGE_LOOP('',(#1076,#1077,#1078,#1079));
#4183=EDGE_LOOP('',(#1080,#1081,#1082,#1083));
#4184=EDGE_LOOP('',(#1084,#1085,#1086,#1087));
#4185=EDGE_LOOP('',(#1088,#1089,#1090,#1091));
#4186=EDGE_LOOP('',(#1092,#1093,#1094,#1095));
#4187=EDGE_LOOP('',(#1096,#1097,#1098,#1099));
#4188=EDGE_LOOP('',(#1100,#1101,#1102,#1103));
#4189=EDGE_LOOP('',(#1104,#1105,#1106,#1107));
#4190=EDGE_LOOP('',(#1108,#1109,#1110,#1111));
#4191=EDGE_LOOP('',(#1112,#1113,#1114,#1115));
#4192=EDGE_LOOP('',(#1116,#1117,#1118,#1119));
#4193=EDGE_LOOP('',(#1120,#1121,#1122,#1123));
#4194=EDGE_LOOP('',(#1124,#1125,#1126,#1127));
#4195=EDGE_LOOP('',(#1128,#1129,#1130,#1131));
#4196=EDGE_LOOP('',(#1132,#1133,#1134,#1135));
#4197=EDGE_LOOP('',(#1136,#1137,#1138,#1139));
#4198=EDGE_LOOP('',(#1140,#1141,#1142,#1143));
#4199=EDGE_LOOP('',(#1144,#1145,#1146,#1147));
#4200=EDGE_LOOP('',(#1148,#1149,#1150,#1151));
#4201=EDGE_LOOP('',(#1152,#1153,#1154,#1155));
#4202=EDGE_LOOP('',(#1156,#1157,#1158,#1159));
#4203=EDGE_LOOP('',(#1160,#1161,#1162,#1163));
#4204=EDGE_LOOP('',(#1164,#1165,#1166,#1167));
#4205=EDGE_LOOP('',(#1168,#1169,#1170,#1171));
#4206=EDGE_LOOP('',(#1172,#1173,#1174,#1175));
#4207=EDGE_LOOP('',(#1176,#1177,#1178,#1179));
#4208=EDGE_LOOP('',(#1180,#1181,#1182,#1183));
#4209=EDGE_LOOP('',(#1184,#1185,#1186,#1187));
#4210=EDGE_LOOP('',(#1188,#1189,#1190,#1191));
#4211=EDGE_LOOP('',(#1192,#1193,#1194,#1195));
#4212=EDGE_LOOP('',(#1196,#1197,#1198,#1199));
#4213=EDGE_LOOP('',(#1200,#1201,#1202,#1203));
#4214=EDGE_LOOP('',(#1204,#1205,#1206,#1207));
#4215=EDGE_LOOP('',(#1208,#1209,#1210,#1211));
#4216=EDGE_LOOP('',(#1212,#1213,#1214,#1215));
#4217=EDGE_LOOP('',(#1216,#1217,#1218,#1219));
#4218=EDGE_LOOP('',(#1220,#1221,#1222,#1223));
#4219=EDGE_LOOP('',(#1224,#1225,#1226,#1227));
#4220=EDGE_LOOP('',(#1228,#1229,#1230,#1231));
#4221=EDGE_LOOP('',(#1232,#1233,#1234,#1235));
#4222=EDGE_LOOP('',(#1236,#1237,#1238,#1239,#1240));
#4223=EDGE_LOOP('',(#1241,#1242,#1243,#1244,#1245,#1246));
#4224=EDGE_LOOP('',(#1247,#1248,#1249,#1250,#1251));
#4225=EDGE_LOOP('',(#1252,#1253,#1254,#1255));
#4226=EDGE_LOOP('',(#1256,#1257,#1258,#1259,#1260));
#4227=EDGE_LOOP('',(#1261,#1262,#1263,#1264));
#4228=EDGE_LOOP('',(#1265,#1266,#1267,#1268,#1269));
#4229=EDGE_LOOP('',(#1270,#1271,#1272,#1273,#1274,#1275));
#4230=EDGE_LOOP('',(#1276,#1277,#1278,#1279));
#4231=EDGE_LOOP('',(#1280,#1281,#1282,#1283));
#4232=EDGE_LOOP('',(#1284,#1285,#1286,#1287));
#4233=EDGE_LOOP('',(#1288,#1289,#1290,#1291));
#4234=EDGE_LOOP('',(#1292,#1293,#1294,#1295));
#4235=EDGE_LOOP('',(#1296,#1297,#1298,#1299,#1300,#1301));
#4236=EDGE_LOOP('',(#1302,#1303,#1304,#1305));
#4237=EDGE_LOOP('',(#1306,#1307,#1308,#1309,#1310,#1311));
#4238=EDGE_LOOP('',(#1312,#1313,#1314,#1315));
#4239=EDGE_LOOP('',(#1316,#1317,#1318,#1319));
#4240=EDGE_LOOP('',(#1320,#1321,#1322,#1323));
#4241=EDGE_LOOP('',(#1324,#1325,#1326,#1327));
#4242=EDGE_LOOP('',(#1328,#1329,#1330,#1331));
#4243=EDGE_LOOP('',(#1332,#1333,#1334,#1335,#1336,#1337,#1338,#1339));
#4244=EDGE_LOOP('',(#1340));
#4245=EDGE_LOOP('',(#1341));
#4246=EDGE_LOOP('',(#1342));
#4247=EDGE_LOOP('',(#1343));
#4248=EDGE_LOOP('',(#1344));
#4249=EDGE_LOOP('',(#1345));
#4250=EDGE_LOOP('',(#1346,#1347,#1348,#1349,#1350,#1351));
#4251=EDGE_LOOP('',(#1352,#1353,#1354,#1355,#1356,#1357));
#4252=EDGE_LOOP('',(#1358,#1359,#1360,#1361,#1362,#1363));
#4253=EDGE_LOOP('',(#1364,#1365,#1366,#1367));
#4254=EDGE_LOOP('',(#1368,#1369,#1370,#1371,#1372,#1373,#1374,#1375,#1376,
#1377,#1378,#1379));
#4255=EDGE_LOOP('',(#1380,#1381,#1382,#1383));
#4256=EDGE_LOOP('',(#1384,#1385,#1386,#1387));
#4257=EDGE_LOOP('',(#1388,#1389,#1390,#1391));
#4258=EDGE_LOOP('',(#1392,#1393,#1394,#1395));
#4259=EDGE_LOOP('',(#1396,#1397,#1398,#1399,#1400));
#4260=EDGE_LOOP('',(#1401,#1402,#1403,#1404,#1405));
#4261=EDGE_LOOP('',(#1406));
#4262=EDGE_LOOP('',(#1407,#1408,#1409,#1410));
#4263=EDGE_LOOP('',(#1411));
#4264=EDGE_LOOP('',(#1412));
#4265=EDGE_LOOP('',(#1413));
#4266=EDGE_LOOP('',(#1414,#1415,#1416,#1417,#1418,#1419,#1420,#1421));
#4267=EDGE_LOOP('',(#1422));
#4268=EDGE_LOOP('',(#1423,#1424,#1425,#1426,#1427,#1428,#1429,#1430));
#4269=EDGE_LOOP('',(#1431));
#4270=EDGE_LOOP('',(#1432));
#4271=EDGE_LOOP('',(#1433));
#4272=EDGE_LOOP('',(#1434,#1435,#1436,#1437));
#4273=EDGE_LOOP('',(#1438));
#4274=EDGE_LOOP('',(#1439,#1440,#1441,#1442));
#4275=EDGE_LOOP('',(#1443));
#4276=EDGE_LOOP('',(#1444,#1445,#1446,#1447));
#4277=EDGE_LOOP('',(#1448,#1449,#1450,#1451));
#4278=EDGE_LOOP('',(#1452,#1453,#1454,#1455));
#4279=EDGE_LOOP('',(#1456,#1457,#1458,#1459));
#4280=EDGE_LOOP('',(#1460));
#4281=EDGE_LOOP('',(#1461));
#4282=EDGE_LOOP('',(#1462));
#4283=EDGE_LOOP('',(#1463));
#4284=EDGE_LOOP('',(#1464));
#4285=EDGE_LOOP('',(#1465));
#4286=EDGE_LOOP('',(#1466));
#4287=EDGE_LOOP('',(#1467));
#4288=EDGE_LOOP('',(#1468));
#4289=EDGE_LOOP('',(#1469));
#4290=EDGE_LOOP('',(#1470));
#4291=EDGE_LOOP('',(#1471));
#4292=EDGE_LOOP('',(#1472));
#4293=EDGE_LOOP('',(#1473));
#4294=EDGE_LOOP('',(#1474));
#4295=EDGE_LOOP('',(#1475));
#4296=EDGE_LOOP('',(#1476,#1477,#1478,#1479));
#4297=EDGE_LOOP('',(#1480,#1481,#1482,#1483));
#4298=EDGE_LOOP('',(#1484,#1485,#1486,#1487));
#4299=EDGE_LOOP('',(#1488));
#4300=EDGE_LOOP('',(#1489));
#4301=EDGE_LOOP('',(#1490,#1491,#1492,#1493));
#4302=EDGE_LOOP('',(#1494));
#4303=EDGE_LOOP('',(#1495));
#4304=EDGE_LOOP('',(#1496));
#4305=EDGE_LOOP('',(#1497));
#4306=EDGE_LOOP('',(#1498));
#4307=EDGE_LOOP('',(#1499));
#4308=EDGE_LOOP('',(#1500));
#4309=EDGE_LOOP('',(#1501));
#4310=EDGE_LOOP('',(#1502));
#4311=EDGE_LOOP('',(#1503));
#4312=EDGE_LOOP('',(#1504));
#4313=EDGE_LOOP('',(#1505));
#4314=EDGE_LOOP('',(#1506,#1507,#1508,#1509));
#4315=EDGE_LOOP('',(#1510));
#4316=EDGE_LOOP('',(#1511));
#4317=EDGE_LOOP('',(#1512));
#4318=EDGE_LOOP('',(#1513));
#4319=EDGE_LOOP('',(#1514));
#4320=EDGE_LOOP('',(#1515));
#4321=EDGE_LOOP('',(#1516,#1517,#1518,#1519));
#4322=EDGE_LOOP('',(#1520));
#4323=EDGE_LOOP('',(#1521));
#4324=EDGE_LOOP('',(#1522));
#4325=EDGE_LOOP('',(#1523));
#4326=EDGE_LOOP('',(#1524));
#4327=EDGE_LOOP('',(#1525));
#4328=EDGE_LOOP('',(#1526));
#4329=EDGE_LOOP('',(#1527));
#4330=EDGE_LOOP('',(#1528));
#4331=EDGE_LOOP('',(#1529));
#4332=EDGE_LOOP('',(#1530));
#4333=EDGE_LOOP('',(#1531));
#4334=EDGE_LOOP('',(#1532));
#4335=EDGE_LOOP('',(#1533));
#4336=EDGE_LOOP('',(#1534));
#4337=EDGE_LOOP('',(#1535));
#4338=EDGE_LOOP('',(#1536));
#4339=EDGE_LOOP('',(#1537));
#4340=EDGE_LOOP('',(#1538));
#4341=EDGE_LOOP('',(#1539));
#4342=EDGE_LOOP('',(#1540));
#4343=EDGE_LOOP('',(#1541));
#4344=EDGE_LOOP('',(#1542));
#4345=EDGE_LOOP('',(#1543));
#4346=EDGE_LOOP('',(#1544,#1545,#1546,#1547,#1548,#1549,#1550,#1551,#1552,
#1553,#1554,#1555,#1556,#1557,#1558,#1559,#1560,#1561,#1562,#1563,#1564,
#1565,#1566,#1567,#1568,#1569,#1570,#1571,#1572,#1573,#1574,#1575,#1576,
#1577,#1578,#1579,#1580,#1581,#1582,#1583,#1584,#1585,#1586,#1587,#1588,
#1589,#1590,#1591,#1592,#1593,#1594,#1595,#1596,#1597,#1598,#1599,#1600,
#1601,#1602,#1603,#1604,#1605,#1606,#1607,#1608,#1609,#1610,#1611,#1612,
#1613,#1614,#1615,#1616,#1617,#1618,#1619,#1620,#1621,#1622,#1623,#1624,
#1625,#1626,#1627,#1628,#1629,#1630,#1631));
#4347=EDGE_LOOP('',(#1632));
#4348=EDGE_LOOP('',(#1633,#1634,#1635,#1636));
#4349=EDGE_LOOP('',(#1637,#1638,#1639,#1640));
#4350=EDGE_LOOP('',(#1641,#1642,#1643,#1644));
#4351=EDGE_LOOP('',(#1645,#1646,#1647,#1648));
#4352=EDGE_LOOP('',(#1649,#1650,#1651,#1652));
#4353=EDGE_LOOP('',(#1653,#1654,#1655,#1656));
#4354=EDGE_LOOP('',(#1657,#1658,#1659,#1660));
#4355=EDGE_LOOP('',(#1661,#1662,#1663,#1664));
#4356=EDGE_LOOP('',(#1665,#1666,#1667,#1668));
#4357=EDGE_LOOP('',(#1669,#1670,#1671,#1672));
#4358=EDGE_LOOP('',(#1673,#1674,#1675,#1676));
#4359=EDGE_LOOP('',(#1677,#1678,#1679,#1680));
#4360=EDGE_LOOP('',(#1681,#1682,#1683,#1684));
#4361=EDGE_LOOP('',(#1685,#1686,#1687,#1688));
#4362=EDGE_LOOP('',(#1689,#1690,#1691,#1692));
#4363=EDGE_LOOP('',(#1693,#1694,#1695,#1696));
#4364=EDGE_LOOP('',(#1697,#1698,#1699,#1700));
#4365=EDGE_LOOP('',(#1701,#1702,#1703,#1704));
#4366=EDGE_LOOP('',(#1705,#1706,#1707,#1708));
#4367=EDGE_LOOP('',(#1709,#1710,#1711,#1712));
#4368=EDGE_LOOP('',(#1713,#1714,#1715,#1716));
#4369=EDGE_LOOP('',(#1717));
#4370=EDGE_LOOP('',(#1718,#1719,#1720,#1721,#1722,#1723,#1724,#1725,#1726,
#1727,#1728,#1729,#1730,#1731,#1732,#1733,#1734,#1735,#1736,#1737,#1738,
#1739,#1740,#1741,#1742,#1743,#1744,#1745,#1746,#1747,#1748,#1749,#1750,
#1751,#1752,#1753,#1754,#1755,#1756,#1757,#1758,#1759,#1760,#1761,#1762,
#1763,#1764,#1765,#1766,#1767,#1768,#1769,#1770,#1771,#1772,#1773,#1774,
#1775,#1776,#1777,#1778,#1779,#1780,#1781,#1782,#1783,#1784,#1785,#1786,
#1787,#1788,#1789,#1790,#1791,#1792,#1793,#1794,#1795,#1796,#1797,#1798,
#1799,#1800,#1801,#1802,#1803,#1804,#1805));
#4371=EDGE_LOOP('',(#1806,#1807,#1808,#1809));
#4372=EDGE_LOOP('',(#1810,#1811,#1812,#1813));
#4373=EDGE_LOOP('',(#1814,#1815,#1816,#1817));
#4374=EDGE_LOOP('',(#1818,#1819,#1820,#1821));
#4375=EDGE_LOOP('',(#1822,#1823,#1824,#1825));
#4376=EDGE_LOOP('',(#1826,#1827,#1828,#1829));
#4377=EDGE_LOOP('',(#1830,#1831,#1832,#1833));
#4378=EDGE_LOOP('',(#1834,#1835,#1836,#1837));
#4379=EDGE_LOOP('',(#1838,#1839,#1840,#1841));
#4380=EDGE_LOOP('',(#1842,#1843,#1844,#1845));
#4381=EDGE_LOOP('',(#1846,#1847,#1848,#1849));
#4382=EDGE_LOOP('',(#1850,#1851,#1852,#1853));
#4383=EDGE_LOOP('',(#1854,#1855,#1856,#1857));
#4384=EDGE_LOOP('',(#1858,#1859,#1860,#1861));
#4385=EDGE_LOOP('',(#1862,#1863,#1864,#1865));
#4386=EDGE_LOOP('',(#1866,#1867,#1868,#1869));
#4387=EDGE_LOOP('',(#1870,#1871,#1872,#1873));
#4388=EDGE_LOOP('',(#1874,#1875,#1876,#1877));
#4389=EDGE_LOOP('',(#1878,#1879,#1880,#1881));
#4390=EDGE_LOOP('',(#1882,#1883,#1884,#1885));
#4391=EDGE_LOOP('',(#1886,#1887,#1888,#1889));
#4392=EDGE_LOOP('',(#1890,#1891,#1892,#1893));
#4393=EDGE_LOOP('',(#1894,#1895,#1896,#1897));
#4394=EDGE_LOOP('',(#1898,#1899,#1900,#1901));
#4395=EDGE_LOOP('',(#1902,#1903,#1904,#1905));
#4396=EDGE_LOOP('',(#1906,#1907,#1908,#1909));
#4397=EDGE_LOOP('',(#1910,#1911,#1912,#1913));
#4398=EDGE_LOOP('',(#1914,#1915,#1916,#1917));
#4399=EDGE_LOOP('',(#1918,#1919,#1920,#1921));
#4400=EDGE_LOOP('',(#1922,#1923,#1924,#1925));
#4401=EDGE_LOOP('',(#1926,#1927,#1928,#1929));
#4402=EDGE_LOOP('',(#1930,#1931,#1932,#1933));
#4403=EDGE_LOOP('',(#1934,#1935,#1936,#1937));
#4404=EDGE_LOOP('',(#1938,#1939,#1940,#1941));
#4405=EDGE_LOOP('',(#1942,#1943,#1944,#1945));
#4406=EDGE_LOOP('',(#1946,#1947,#1948,#1949));
#4407=EDGE_LOOP('',(#1950,#1951,#1952,#1953));
#4408=EDGE_LOOP('',(#1954,#1955,#1956,#1957));
#4409=EDGE_LOOP('',(#1958,#1959,#1960,#1961));
#4410=EDGE_LOOP('',(#1962,#1963,#1964,#1965));
#4411=EDGE_LOOP('',(#1966,#1967,#1968,#1969));
#4412=EDGE_LOOP('',(#1970,#1971,#1972,#1973));
#4413=EDGE_LOOP('',(#1974,#1975,#1976,#1977));
#4414=EDGE_LOOP('',(#1978,#1979,#1980,#1981));
#4415=EDGE_LOOP('',(#1982,#1983,#1984,#1985));
#4416=EDGE_LOOP('',(#1986,#1987,#1988,#1989));
#4417=EDGE_LOOP('',(#1990,#1991,#1992,#1993));
#4418=EDGE_LOOP('',(#1994,#1995,#1996,#1997));
#4419=EDGE_LOOP('',(#1998,#1999,#2000,#2001));
#4420=EDGE_LOOP('',(#2002,#2003,#2004,#2005));
#4421=EDGE_LOOP('',(#2006,#2007,#2008,#2009));
#4422=EDGE_LOOP('',(#2010,#2011,#2012,#2013));
#4423=EDGE_LOOP('',(#2014,#2015,#2016,#2017));
#4424=EDGE_LOOP('',(#2018,#2019,#2020,#2021));
#4425=EDGE_LOOP('',(#2022,#2023,#2024,#2025));
#4426=EDGE_LOOP('',(#2026,#2027,#2028,#2029));
#4427=EDGE_LOOP('',(#2030,#2031,#2032,#2033));
#4428=EDGE_LOOP('',(#2034,#2035,#2036,#2037));
#4429=EDGE_LOOP('',(#2038,#2039,#2040,#2041));
#4430=EDGE_LOOP('',(#2042,#2043,#2044,#2045));
#4431=EDGE_LOOP('',(#2046,#2047,#2048,#2049));
#4432=EDGE_LOOP('',(#2050,#2051,#2052,#2053));
#4433=EDGE_LOOP('',(#2054,#2055,#2056,#2057));
#4434=EDGE_LOOP('',(#2058,#2059,#2060,#2061));
#4435=EDGE_LOOP('',(#2062,#2063,#2064,#2065));
#4436=EDGE_LOOP('',(#2066,#2067,#2068,#2069));
#4437=EDGE_LOOP('',(#2070,#2071,#2072,#2073));
#4438=EDGE_LOOP('',(#2074));
#4439=EDGE_LOOP('',(#2075));
#4440=EDGE_LOOP('',(#2076));
#4441=EDGE_LOOP('',(#2077));
#4442=EDGE_LOOP('',(#2078));
#4443=EDGE_LOOP('',(#2079));
#4444=EDGE_LOOP('',(#2080));
#4445=EDGE_LOOP('',(#2081));
#4446=EDGE_LOOP('',(#2082));
#4447=EDGE_LOOP('',(#2083));
#4448=EDGE_LOOP('',(#2084));
#4449=EDGE_LOOP('',(#2085));
#4450=EDGE_LOOP('',(#2086));
#4451=EDGE_LOOP('',(#2087));
#4452=EDGE_LOOP('',(#2088,#2089,#2090,#2091));
#4453=EDGE_LOOP('',(#2092,#2093,#2094,#2095));
#4454=EDGE_LOOP('',(#2096,#2097,#2098,#2099));
#4455=EDGE_LOOP('',(#2100,#2101,#2102,#2103));
#4456=EDGE_LOOP('',(#2104));
#4457=EDGE_LOOP('',(#2105,#2106,#2107,#2108));
#4458=EDGE_LOOP('',(#2109));
#4459=EDGE_LOOP('',(#2110,#2111,#2112,#2113));
#4460=EDGE_LOOP('',(#2114));
#4461=EDGE_LOOP('',(#2115));
#4462=EDGE_LOOP('',(#2116,#2117,#2118,#2119));
#4463=EDGE_LOOP('',(#2120,#2121,#2122,#2123));
#4464=EDGE_LOOP('',(#2124,#2125,#2126,#2127));
#4465=EDGE_LOOP('',(#2128,#2129,#2130,#2131));
#4466=EDGE_LOOP('',(#2132,#2133,#2134,#2135));
#4467=EDGE_LOOP('',(#2136,#2137,#2138,#2139));
#4468=EDGE_LOOP('',(#2140,#2141,#2142,#2143));
#4469=EDGE_LOOP('',(#2144,#2145,#2146,#2147));
#4470=EDGE_LOOP('',(#2148,#2149,#2150,#2151));
#4471=EDGE_LOOP('',(#2152,#2153,#2154,#2155));
#4472=EDGE_LOOP('',(#2156,#2157,#2158,#2159));
#4473=EDGE_LOOP('',(#2160,#2161,#2162,#2163));
#4474=EDGE_LOOP('',(#2164));
#4475=EDGE_LOOP('',(#2165,#2166,#2167,#2168));
#4476=EDGE_LOOP('',(#2169));
#4477=EDGE_LOOP('',(#2170,#2171,#2172,#2173));
#4478=EDGE_LOOP('',(#2174));
#4479=EDGE_LOOP('',(#2175));
#4480=EDGE_LOOP('',(#2176,#2177,#2178,#2179));
#4481=EDGE_LOOP('',(#2180,#2181,#2182,#2183));
#4482=EDGE_LOOP('',(#2184,#2185,#2186,#2187));
#4483=EDGE_LOOP('',(#2188,#2189,#2190,#2191));
#4484=EDGE_LOOP('',(#2192));
#4485=EDGE_LOOP('',(#2193));
#4486=EDGE_LOOP('',(#2194));
#4487=EDGE_LOOP('',(#2195));
#4488=EDGE_LOOP('',(#2196));
#4489=EDGE_LOOP('',(#2197));
#4490=EDGE_LOOP('',(#2198));
#4491=EDGE_LOOP('',(#2199));
#4492=EDGE_LOOP('',(#2200));
#4493=EDGE_LOOP('',(#2201));
#4494=EDGE_LOOP('',(#2202));
#4495=EDGE_LOOP('',(#2203));
#4496=EDGE_LOOP('',(#2204));
#4497=EDGE_LOOP('',(#2205));
#4498=EDGE_LOOP('',(#2206));
#4499=EDGE_LOOP('',(#2207));
#4500=EDGE_LOOP('',(#2208));
#4501=EDGE_LOOP('',(#2209));
#4502=EDGE_LOOP('',(#2210));
#4503=EDGE_LOOP('',(#2211));
#4504=EDGE_LOOP('',(#2212));
#4505=EDGE_LOOP('',(#2213));
#4506=EDGE_LOOP('',(#2214));
#4507=EDGE_LOOP('',(#2215));
#4508=EDGE_LOOP('',(#2216));
#4509=EDGE_LOOP('',(#2217));
#4510=EDGE_LOOP('',(#2218));
#4511=EDGE_LOOP('',(#2219));
#4512=EDGE_LOOP('',(#2220));
#4513=EDGE_LOOP('',(#2221));
#4514=EDGE_LOOP('',(#2222));
#4515=EDGE_LOOP('',(#2223));
#4516=EDGE_LOOP('',(#2224));
#4517=EDGE_LOOP('',(#2225));
#4518=EDGE_LOOP('',(#2226));
#4519=EDGE_LOOP('',(#2227));
#4520=EDGE_LOOP('',(#2228,#2229,#2230,#2231,#2232,#2233,#2234,#2235,#2236,
#2237,#2238));
#4521=EDGE_LOOP('',(#2239));
#4522=EDGE_LOOP('',(#2240,#2241,#2242,#2243,#2244,#2245,#2246,#2247,#2248,
#2249,#2250));
#4523=EDGE_LOOP('',(#2251));
#4524=EDGE_LOOP('',(#2252,#2253,#2254,#2255));
#4525=EDGE_LOOP('',(#2256,#2257,#2258,#2259));
#4526=EDGE_LOOP('',(#2260,#2261,#2262,#2263));
#4527=EDGE_LOOP('',(#2264,#2265,#2266,#2267));
#4528=EDGE_LOOP('',(#2268,#2269,#2270,#2271));
#4529=EDGE_LOOP('',(#2272,#2273,#2274,#2275));
#4530=EDGE_LOOP('',(#2276,#2277,#2278,#2279));
#4531=EDGE_LOOP('',(#2280,#2281,#2282,#2283));
#4532=EDGE_LOOP('',(#2284,#2285,#2286,#2287));
#4533=EDGE_LOOP('',(#2288,#2289,#2290,#2291));
#4534=EDGE_LOOP('',(#2292,#2293,#2294,#2295));
#4535=EDGE_LOOP('',(#2296));
#4536=EDGE_LOOP('',(#2297));
#4537=EDGE_LOOP('',(#2298,#2299));
#4538=EDGE_LOOP('',(#2300,#2301,#2302,#2303));
#4539=EDGE_LOOP('',(#2304));
#4540=EDGE_LOOP('',(#2305));
#4541=EDGE_LOOP('',(#2306));
#4542=EDGE_LOOP('',(#2307,#2308));
#4543=EDGE_LOOP('',(#2309,#2310,#2311,#2312,#2313,#2314,#2315,#2316));
#4544=EDGE_LOOP('',(#2317));
#4545=EDGE_LOOP('',(#2318));
#4546=EDGE_LOOP('',(#2319));
#4547=EDGE_LOOP('',(#2320));
#4548=EDGE_LOOP('',(#2321));
#4549=EDGE_LOOP('',(#2322,#2323,#2324,#2325));
#4550=EDGE_LOOP('',(#2326,#2327,#2328,#2329));
#4551=EDGE_LOOP('',(#2330,#2331,#2332,#2333,#2334,#2335));
#4552=EDGE_LOOP('',(#2336,#2337,#2338,#2339,#2340,#2341));
#4553=EDGE_LOOP('',(#2342));
#4554=EDGE_LOOP('',(#2343));
#4555=FACE_BOUND('',#4107,.T.);
#4556=FACE_BOUND('',#4108,.T.);
#4557=FACE_BOUND('',#4109,.T.);
#4558=FACE_BOUND('',#4110,.T.);
#4559=FACE_BOUND('',#4111,.T.);
#4560=FACE_BOUND('',#4112,.T.);
#4561=FACE_BOUND('',#4113,.T.);
#4562=FACE_BOUND('',#4114,.T.);
#4563=FACE_BOUND('',#4115,.T.);
#4564=FACE_BOUND('',#4116,.T.);
#4565=FACE_BOUND('',#4117,.T.);
#4566=FACE_BOUND('',#4118,.T.);
#4567=FACE_BOUND('',#4119,.T.);
#4568=FACE_BOUND('',#4120,.T.);
#4569=FACE_BOUND('',#4121,.T.);
#4570=FACE_BOUND('',#4122,.T.);
#4571=FACE_BOUND('',#4123,.T.);
#4572=FACE_BOUND('',#4124,.T.);
#4573=FACE_BOUND('',#4125,.T.);
#4574=FACE_BOUND('',#4126,.T.);
#4575=FACE_BOUND('',#4127,.T.);
#4576=FACE_BOUND('',#4128,.T.);
#4577=FACE_BOUND('',#4129,.T.);
#4578=FACE_BOUND('',#4130,.T.);
#4579=FACE_BOUND('',#4131,.T.);
#4580=FACE_BOUND('',#4132,.T.);
#4581=FACE_BOUND('',#4133,.T.);
#4582=FACE_BOUND('',#4134,.T.);
#4583=FACE_BOUND('',#4135,.T.);
#4584=FACE_BOUND('',#4136,.T.);
#4585=FACE_BOUND('',#4137,.T.);
#4586=FACE_BOUND('',#4138,.T.);
#4587=FACE_BOUND('',#4139,.T.);
#4588=FACE_BOUND('',#4140,.T.);
#4589=FACE_BOUND('',#4141,.T.);
#4590=FACE_BOUND('',#4142,.T.);
#4591=FACE_BOUND('',#4143,.T.);
#4592=FACE_BOUND('',#4144,.T.);
#4593=FACE_BOUND('',#4145,.T.);
#4594=FACE_BOUND('',#4146,.T.);
#4595=FACE_BOUND('',#4147,.T.);
#4596=FACE_BOUND('',#4148,.T.);
#4597=FACE_BOUND('',#4149,.T.);
#4598=FACE_BOUND('',#4150,.T.);
#4599=FACE_BOUND('',#4151,.T.);
#4600=FACE_BOUND('',#4152,.T.);
#4601=FACE_BOUND('',#4153,.T.);
#4602=FACE_BOUND('',#4154,.T.);
#4603=FACE_BOUND('',#4155,.T.);
#4604=FACE_BOUND('',#4156,.T.);
#4605=FACE_BOUND('',#4157,.T.);
#4606=FACE_BOUND('',#4158,.T.);
#4607=FACE_BOUND('',#4159,.T.);
#4608=FACE_BOUND('',#4160,.T.);
#4609=FACE_BOUND('',#4161,.T.);
#4610=FACE_BOUND('',#4162,.T.);
#4611=FACE_BOUND('',#4163,.T.);
#4612=FACE_BOUND('',#4164,.T.);
#4613=FACE_BOUND('',#4165,.T.);
#4614=FACE_BOUND('',#4166,.T.);
#4615=FACE_BOUND('',#4167,.T.);
#4616=FACE_BOUND('',#4168,.T.);
#4617=FACE_BOUND('',#4169,.T.);
#4618=FACE_BOUND('',#4170,.T.);
#4619=FACE_BOUND('',#4171,.T.);
#4620=FACE_BOUND('',#4172,.T.);
#4621=FACE_BOUND('',#4173,.T.);
#4622=FACE_BOUND('',#4174,.T.);
#4623=FACE_BOUND('',#4175,.T.);
#4624=FACE_BOUND('',#4176,.T.);
#4625=FACE_BOUND('',#4177,.T.);
#4626=FACE_BOUND('',#4178,.T.);
#4627=FACE_BOUND('',#4179,.T.);
#4628=FACE_BOUND('',#4180,.T.);
#4629=FACE_BOUND('',#4181,.T.);
#4630=FACE_BOUND('',#4182,.T.);
#4631=FACE_BOUND('',#4183,.T.);
#4632=FACE_BOUND('',#4184,.T.);
#4633=FACE_BOUND('',#4185,.T.);
#4634=FACE_BOUND('',#4186,.T.);
#4635=FACE_BOUND('',#4187,.T.);
#4636=FACE_BOUND('',#4188,.T.);
#4637=FACE_BOUND('',#4189,.T.);
#4638=FACE_BOUND('',#4190,.T.);
#4639=FACE_BOUND('',#4191,.T.);
#4640=FACE_BOUND('',#4192,.T.);
#4641=FACE_BOUND('',#4193,.T.);
#4642=FACE_BOUND('',#4194,.T.);
#4643=FACE_BOUND('',#4195,.T.);
#4644=FACE_BOUND('',#4196,.T.);
#4645=FACE_BOUND('',#4197,.T.);
#4646=FACE_BOUND('',#4198,.T.);
#4647=FACE_BOUND('',#4199,.T.);
#4648=FACE_BOUND('',#4200,.T.);
#4649=FACE_BOUND('',#4201,.T.);
#4650=FACE_BOUND('',#4202,.T.);
#4651=FACE_BOUND('',#4203,.T.);
#4652=FACE_BOUND('',#4204,.T.);
#4653=FACE_BOUND('',#4205,.T.);
#4654=FACE_BOUND('',#4206,.T.);
#4655=FACE_BOUND('',#4207,.T.);
#4656=FACE_BOUND('',#4208,.T.);
#4657=FACE_BOUND('',#4209,.T.);
#4658=FACE_BOUND('',#4210,.T.);
#4659=FACE_BOUND('',#4211,.T.);
#4660=FACE_BOUND('',#4212,.T.);
#4661=FACE_BOUND('',#4213,.T.);
#4662=FACE_BOUND('',#4214,.T.);
#4663=FACE_BOUND('',#4215,.T.);
#4664=FACE_BOUND('',#4216,.T.);
#4665=FACE_BOUND('',#4217,.T.);
#4666=FACE_BOUND('',#4218,.T.);
#4667=FACE_BOUND('',#4219,.T.);
#4668=FACE_BOUND('',#4220,.T.);
#4669=FACE_BOUND('',#4221,.T.);
#4670=FACE_BOUND('',#4222,.T.);
#4671=FACE_BOUND('',#4223,.T.);
#4672=FACE_BOUND('',#4224,.T.);
#4673=FACE_BOUND('',#4225,.T.);
#4674=FACE_BOUND('',#4226,.T.);
#4675=FACE_BOUND('',#4227,.T.);
#4676=FACE_BOUND('',#4228,.T.);
#4677=FACE_BOUND('',#4229,.T.);
#4678=FACE_BOUND('',#4230,.T.);
#4679=FACE_BOUND('',#4231,.T.);
#4680=FACE_BOUND('',#4232,.T.);
#4681=FACE_BOUND('',#4233,.T.);
#4682=FACE_BOUND('',#4234,.T.);
#4683=FACE_BOUND('',#4235,.T.);
#4684=FACE_BOUND('',#4236,.T.);
#4685=FACE_BOUND('',#4237,.T.);
#4686=FACE_BOUND('',#4238,.T.);
#4687=FACE_BOUND('',#4239,.T.);
#4688=FACE_BOUND('',#4240,.T.);
#4689=FACE_BOUND('',#4241,.T.);
#4690=FACE_BOUND('',#4242,.T.);
#4691=FACE_BOUND('',#4243,.T.);
#4692=FACE_BOUND('',#4244,.T.);
#4693=FACE_BOUND('',#4245,.T.);
#4694=FACE_BOUND('',#4246,.T.);
#4695=FACE_BOUND('',#4247,.T.);
#4696=FACE_BOUND('',#4248,.T.);
#4697=FACE_BOUND('',#4249,.T.);
#4698=FACE_BOUND('',#4250,.T.);
#4699=FACE_BOUND('',#4251,.T.);
#4700=FACE_BOUND('',#4252,.T.);
#4701=FACE_BOUND('',#4253,.T.);
#4702=FACE_BOUND('',#4254,.T.);
#4703=FACE_BOUND('',#4255,.T.);
#4704=FACE_BOUND('',#4256,.T.);
#4705=FACE_BOUND('',#4257,.T.);
#4706=FACE_BOUND('',#4258,.T.);
#4707=FACE_BOUND('',#4259,.T.);
#4708=FACE_BOUND('',#4260,.T.);
#4709=FACE_BOUND('',#4261,.T.);
#4710=FACE_BOUND('',#4262,.T.);
#4711=FACE_BOUND('',#4263,.T.);
#4712=FACE_BOUND('',#4264,.T.);
#4713=FACE_BOUND('',#4265,.T.);
#4714=FACE_BOUND('',#4266,.T.);
#4715=FACE_BOUND('',#4267,.T.);
#4716=FACE_BOUND('',#4268,.T.);
#4717=FACE_BOUND('',#4269,.T.);
#4718=FACE_BOUND('',#4270,.T.);
#4719=FACE_BOUND('',#4271,.T.);
#4720=FACE_BOUND('',#4272,.T.);
#4721=FACE_BOUND('',#4273,.T.);
#4722=FACE_BOUND('',#4274,.T.);
#4723=FACE_BOUND('',#4275,.T.);
#4724=FACE_BOUND('',#4276,.T.);
#4725=FACE_BOUND('',#4277,.T.);
#4726=FACE_BOUND('',#4278,.T.);
#4727=FACE_BOUND('',#4279,.T.);
#4728=FACE_BOUND('',#4280,.T.);
#4729=FACE_BOUND('',#4281,.T.);
#4730=FACE_BOUND('',#4282,.T.);
#4731=FACE_BOUND('',#4283,.T.);
#4732=FACE_BOUND('',#4284,.T.);
#4733=FACE_BOUND('',#4285,.T.);
#4734=FACE_BOUND('',#4286,.T.);
#4735=FACE_BOUND('',#4287,.T.);
#4736=FACE_BOUND('',#4288,.T.);
#4737=FACE_BOUND('',#4289,.T.);
#4738=FACE_BOUND('',#4290,.T.);
#4739=FACE_BOUND('',#4291,.T.);
#4740=FACE_BOUND('',#4292,.T.);
#4741=FACE_BOUND('',#4293,.T.);
#4742=FACE_BOUND('',#4294,.T.);
#4743=FACE_BOUND('',#4295,.T.);
#4744=FACE_BOUND('',#4296,.T.);
#4745=FACE_BOUND('',#4297,.T.);
#4746=FACE_BOUND('',#4298,.T.);
#4747=FACE_BOUND('',#4299,.T.);
#4748=FACE_BOUND('',#4300,.T.);
#4749=FACE_BOUND('',#4301,.T.);
#4750=FACE_BOUND('',#4302,.T.);
#4751=FACE_BOUND('',#4303,.T.);
#4752=FACE_BOUND('',#4304,.T.);
#4753=FACE_BOUND('',#4305,.T.);
#4754=FACE_BOUND('',#4306,.T.);
#4755=FACE_BOUND('',#4307,.T.);
#4756=FACE_BOUND('',#4308,.T.);
#4757=FACE_BOUND('',#4309,.T.);
#4758=FACE_BOUND('',#4310,.T.);
#4759=FACE_BOUND('',#4311,.T.);
#4760=FACE_BOUND('',#4312,.T.);
#4761=FACE_BOUND('',#4313,.T.);
#4762=FACE_BOUND('',#4314,.T.);
#4763=FACE_BOUND('',#4315,.T.);
#4764=FACE_BOUND('',#4316,.T.);
#4765=FACE_BOUND('',#4317,.T.);
#4766=FACE_BOUND('',#4318,.T.);
#4767=FACE_BOUND('',#4319,.T.);
#4768=FACE_BOUND('',#4320,.T.);
#4769=FACE_BOUND('',#4321,.T.);
#4770=FACE_BOUND('',#4322,.T.);
#4771=FACE_BOUND('',#4323,.T.);
#4772=FACE_BOUND('',#4324,.T.);
#4773=FACE_BOUND('',#4325,.T.);
#4774=FACE_BOUND('',#4326,.T.);
#4775=FACE_BOUND('',#4327,.T.);
#4776=FACE_BOUND('',#4328,.T.);
#4777=FACE_BOUND('',#4329,.T.);
#4778=FACE_BOUND('',#4330,.T.);
#4779=FACE_BOUND('',#4331,.T.);
#4780=FACE_BOUND('',#4332,.T.);
#4781=FACE_BOUND('',#4333,.T.);
#4782=FACE_BOUND('',#4334,.T.);
#4783=FACE_BOUND('',#4335,.T.);
#4784=FACE_BOUND('',#4336,.T.);
#4785=FACE_BOUND('',#4337,.T.);
#4786=FACE_BOUND('',#4338,.T.);
#4787=FACE_BOUND('',#4339,.T.);
#4788=FACE_BOUND('',#4340,.T.);
#4789=FACE_BOUND('',#4341,.T.);
#4790=FACE_BOUND('',#4342,.T.);
#4791=FACE_BOUND('',#4343,.T.);
#4792=FACE_BOUND('',#4344,.T.);
#4793=FACE_BOUND('',#4345,.T.);
#4794=FACE_BOUND('',#4346,.T.);
#4795=FACE_BOUND('',#4347,.T.);
#4796=FACE_BOUND('',#4348,.T.);
#4797=FACE_BOUND('',#4349,.T.);
#4798=FACE_BOUND('',#4350,.T.);
#4799=FACE_BOUND('',#4351,.T.);
#4800=FACE_BOUND('',#4352,.T.);
#4801=FACE_BOUND('',#4353,.T.);
#4802=FACE_BOUND('',#4354,.T.);
#4803=FACE_BOUND('',#4355,.T.);
#4804=FACE_BOUND('',#4356,.T.);
#4805=FACE_BOUND('',#4357,.T.);
#4806=FACE_BOUND('',#4358,.T.);
#4807=FACE_BOUND('',#4359,.T.);
#4808=FACE_BOUND('',#4360,.T.);
#4809=FACE_BOUND('',#4361,.T.);
#4810=FACE_BOUND('',#4362,.T.);
#4811=FACE_BOUND('',#4363,.T.);
#4812=FACE_BOUND('',#4364,.T.);
#4813=FACE_BOUND('',#4365,.T.);
#4814=FACE_BOUND('',#4366,.T.);
#4815=FACE_BOUND('',#4367,.T.);
#4816=FACE_BOUND('',#4368,.T.);
#4817=FACE_BOUND('',#4369,.T.);
#4818=FACE_BOUND('',#4370,.T.);
#4819=FACE_BOUND('',#4371,.T.);
#4820=FACE_BOUND('',#4372,.T.);
#4821=FACE_BOUND('',#4373,.T.);
#4822=FACE_BOUND('',#4374,.T.);
#4823=FACE_BOUND('',#4375,.T.);
#4824=FACE_BOUND('',#4376,.T.);
#4825=FACE_BOUND('',#4377,.T.);
#4826=FACE_BOUND('',#4378,.T.);
#4827=FACE_BOUND('',#4379,.T.);
#4828=FACE_BOUND('',#4380,.T.);
#4829=FACE_BOUND('',#4381,.T.);
#4830=FACE_BOUND('',#4382,.T.);
#4831=FACE_BOUND('',#4383,.T.);
#4832=FACE_BOUND('',#4384,.T.);
#4833=FACE_BOUND('',#4385,.T.);
#4834=FACE_BOUND('',#4386,.T.);
#4835=FACE_BOUND('',#4387,.T.);
#4836=FACE_BOUND('',#4388,.T.);
#4837=FACE_BOUND('',#4389,.T.);
#4838=FACE_BOUND('',#4390,.T.);
#4839=FACE_BOUND('',#4391,.T.);
#4840=FACE_BOUND('',#4392,.T.);
#4841=FACE_BOUND('',#4393,.T.);
#4842=FACE_BOUND('',#4394,.T.);
#4843=FACE_BOUND('',#4395,.T.);
#4844=FACE_BOUND('',#4396,.T.);
#4845=FACE_BOUND('',#4397,.T.);
#4846=FACE_BOUND('',#4398,.T.);
#4847=FACE_BOUND('',#4399,.T.);
#4848=FACE_BOUND('',#4400,.T.);
#4849=FACE_BOUND('',#4401,.T.);
#4850=FACE_BOUND('',#4402,.T.);
#4851=FACE_BOUND('',#4403,.T.);
#4852=FACE_BOUND('',#4404,.T.);
#4853=FACE_BOUND('',#4405,.T.);
#4854=FACE_BOUND('',#4406,.T.);
#4855=FACE_BOUND('',#4407,.T.);
#4856=FACE_BOUND('',#4408,.T.);
#4857=FACE_BOUND('',#4409,.T.);
#4858=FACE_BOUND('',#4410,.T.);
#4859=FACE_BOUND('',#4411,.T.);
#4860=FACE_BOUND('',#4412,.T.);
#4861=FACE_BOUND('',#4413,.T.);
#4862=FACE_BOUND('',#4414,.T.);
#4863=FACE_BOUND('',#4415,.T.);
#4864=FACE_BOUND('',#4416,.T.);
#4865=FACE_BOUND('',#4417,.T.);
#4866=FACE_BOUND('',#4418,.T.);
#4867=FACE_BOUND('',#4419,.T.);
#4868=FACE_BOUND('',#4420,.T.);
#4869=FACE_BOUND('',#4421,.T.);
#4870=FACE_BOUND('',#4422,.T.);
#4871=FACE_BOUND('',#4423,.T.);
#4872=FACE_BOUND('',#4424,.T.);
#4873=FACE_BOUND('',#4425,.T.);
#4874=FACE_BOUND('',#4426,.T.);
#4875=FACE_BOUND('',#4427,.T.);
#4876=FACE_BOUND('',#4428,.T.);
#4877=FACE_BOUND('',#4429,.T.);
#4878=FACE_BOUND('',#4430,.T.);
#4879=FACE_BOUND('',#4431,.T.);
#4880=FACE_BOUND('',#4432,.T.);
#4881=FACE_BOUND('',#4433,.T.);
#4882=FACE_BOUND('',#4434,.T.);
#4883=FACE_BOUND('',#4435,.T.);
#4884=FACE_BOUND('',#4436,.T.);
#4885=FACE_BOUND('',#4437,.T.);
#4886=FACE_BOUND('',#4438,.T.);
#4887=FACE_BOUND('',#4439,.T.);
#4888=FACE_BOUND('',#4440,.T.);
#4889=FACE_BOUND('',#4441,.T.);
#4890=FACE_BOUND('',#4442,.T.);
#4891=FACE_BOUND('',#4443,.T.);
#4892=FACE_BOUND('',#4444,.T.);
#4893=FACE_BOUND('',#4445,.T.);
#4894=FACE_BOUND('',#4446,.T.);
#4895=FACE_BOUND('',#4447,.T.);
#4896=FACE_BOUND('',#4448,.T.);
#4897=FACE_BOUND('',#4449,.T.);
#4898=FACE_BOUND('',#4450,.T.);
#4899=FACE_BOUND('',#4451,.T.);
#4900=FACE_BOUND('',#4452,.T.);
#4901=FACE_BOUND('',#4453,.T.);
#4902=FACE_BOUND('',#4454,.T.);
#4903=FACE_BOUND('',#4455,.T.);
#4904=FACE_BOUND('',#4456,.T.);
#4905=FACE_BOUND('',#4457,.T.);
#4906=FACE_BOUND('',#4458,.T.);
#4907=FACE_BOUND('',#4459,.T.);
#4908=FACE_BOUND('',#4460,.T.);
#4909=FACE_BOUND('',#4461,.T.);
#4910=FACE_BOUND('',#4462,.T.);
#4911=FACE_BOUND('',#4463,.T.);
#4912=FACE_BOUND('',#4464,.T.);
#4913=FACE_BOUND('',#4465,.T.);
#4914=FACE_BOUND('',#4466,.T.);
#4915=FACE_BOUND('',#4467,.T.);
#4916=FACE_BOUND('',#4468,.T.);
#4917=FACE_BOUND('',#4469,.T.);
#4918=FACE_BOUND('',#4470,.T.);
#4919=FACE_BOUND('',#4471,.T.);
#4920=FACE_BOUND('',#4472,.T.);
#4921=FACE_BOUND('',#4473,.T.);
#4922=FACE_BOUND('',#4474,.T.);
#4923=FACE_BOUND('',#4475,.T.);
#4924=FACE_BOUND('',#4476,.T.);
#4925=FACE_BOUND('',#4477,.T.);
#4926=FACE_BOUND('',#4478,.T.);
#4927=FACE_BOUND('',#4479,.T.);
#4928=FACE_BOUND('',#4480,.T.);
#4929=FACE_BOUND('',#4481,.T.);
#4930=FACE_BOUND('',#4482,.T.);
#4931=FACE_BOUND('',#4483,.T.);
#4932=FACE_BOUND('',#4484,.T.);
#4933=FACE_BOUND('',#4485,.T.);
#4934=FACE_BOUND('',#4486,.T.);
#4935=FACE_BOUND('',#4487,.T.);
#4936=FACE_BOUND('',#4488,.T.);
#4937=FACE_BOUND('',#4489,.T.);
#4938=FACE_BOUND('',#4490,.T.);
#4939=FACE_BOUND('',#4491,.T.);
#4940=FACE_BOUND('',#4492,.T.);
#4941=FACE_BOUND('',#4493,.T.);
#4942=FACE_BOUND('',#4494,.T.);
#4943=FACE_BOUND('',#4495,.T.);
#4944=FACE_BOUND('',#4496,.T.);
#4945=FACE_BOUND('',#4497,.T.);
#4946=FACE_BOUND('',#4498,.T.);
#4947=FACE_BOUND('',#4499,.T.);
#4948=FACE_BOUND('',#4500,.T.);
#4949=FACE_BOUND('',#4501,.T.);
#4950=FACE_BOUND('',#4502,.T.);
#4951=FACE_BOUND('',#4503,.T.);
#4952=FACE_BOUND('',#4504,.T.);
#4953=FACE_BOUND('',#4505,.T.);
#4954=FACE_BOUND('',#4506,.T.);
#4955=FACE_BOUND('',#4507,.T.);
#4956=FACE_BOUND('',#4508,.T.);
#4957=FACE_BOUND('',#4509,.T.);
#4958=FACE_BOUND('',#4510,.T.);
#4959=FACE_BOUND('',#4511,.T.);
#4960=FACE_BOUND('',#4512,.T.);
#4961=FACE_BOUND('',#4513,.T.);
#4962=FACE_BOUND('',#4514,.T.);
#4963=FACE_BOUND('',#4515,.T.);
#4964=FACE_BOUND('',#4516,.T.);
#4965=FACE_BOUND('',#4517,.T.);
#4966=FACE_BOUND('',#4518,.T.);
#4967=FACE_BOUND('',#4519,.T.);
#4968=FACE_BOUND('',#4520,.T.);
#4969=FACE_BOUND('',#4521,.T.);
#4970=FACE_BOUND('',#4522,.T.);
#4971=FACE_BOUND('',#4523,.T.);
#4972=FACE_BOUND('',#4524,.T.);
#4973=FACE_BOUND('',#4525,.T.);
#4974=FACE_BOUND('',#4526,.T.);
#4975=FACE_BOUND('',#4527,.T.);
#4976=FACE_BOUND('',#4528,.T.);
#4977=FACE_BOUND('',#4529,.T.);
#4978=FACE_BOUND('',#4530,.T.);
#4979=FACE_BOUND('',#4531,.T.);
#4980=FACE_BOUND('',#4532,.T.);
#4981=FACE_BOUND('',#4533,.T.);
#4982=FACE_BOUND('',#4534,.T.);
#4983=FACE_BOUND('',#4535,.T.);
#4984=FACE_BOUND('',#4536,.T.);
#4985=FACE_BOUND('',#4537,.T.);
#4986=FACE_BOUND('',#4538,.T.);
#4987=FACE_BOUND('',#4539,.T.);
#4988=FACE_BOUND('',#4540,.T.);
#4989=FACE_BOUND('',#4541,.T.);
#4990=FACE_BOUND('',#4542,.T.);
#4991=FACE_BOUND('',#4543,.T.);
#4992=FACE_BOUND('',#4544,.T.);
#4993=FACE_BOUND('',#4545,.T.);
#4994=FACE_BOUND('',#4546,.T.);
#4995=FACE_BOUND('',#4547,.T.);
#4996=FACE_BOUND('',#4548,.T.);
#4997=FACE_BOUND('',#4549,.T.);
#4998=FACE_BOUND('',#4550,.T.);
#4999=FACE_BOUND('',#4551,.T.);
#5000=FACE_BOUND('',#4552,.T.);
#5001=FACE_BOUND('',#4553,.T.);
#5002=FACE_BOUND('',#4554,.T.);
#5003=CYLINDRICAL_SURFACE('',#5705,0.06);
#5004=CYLINDRICAL_SURFACE('',#5708,0.061);
#5005=CYLINDRICAL_SURFACE('',#5718,0.0635);
#5006=CYLINDRICAL_SURFACE('',#5726,0.005);
#5007=CYLINDRICAL_SURFACE('',#5727,0.0015);
#5008=CYLINDRICAL_SURFACE('',#5728,0.0015);
#5009=CYLINDRICAL_SURFACE('',#5729,0.0015);
#5010=CYLINDRICAL_SURFACE('',#5730,0.0015);
#5011=CYLINDRICAL_SURFACE('',#5737,0.00125);
#5012=CYLINDRICAL_SURFACE('',#5758,0.0125);
#5013=CYLINDRICAL_SURFACE('',#5761,0.0125);
#5014=CYLINDRICAL_SURFACE('',#5764,0.0015);
#5015=CYLINDRICAL_SURFACE('',#5868,0.0354217830972575);
#5016=CYLINDRICAL_SURFACE('',#5869,0.005);
#5017=CYLINDRICAL_SURFACE('',#5871,0.00499999999999989);
#5018=CYLINDRICAL_SURFACE('',#5873,0.015);
#5019=CYLINDRICAL_SURFACE('',#5874,0.0015);
#5020=CYLINDRICAL_SURFACE('',#5876,0.0015);
#5021=CYLINDRICAL_SURFACE('',#5878,0.0125);
#5022=CYLINDRICAL_SURFACE('',#5879,0.0125);
#5023=CYLINDRICAL_SURFACE('',#5880,0.0125);
#5024=CYLINDRICAL_SURFACE('',#5881,0.0125);
#5025=CYLINDRICAL_SURFACE('',#5882,0.0125);
#5026=CYLINDRICAL_SURFACE('',#5883,0.0125);
#5027=CYLINDRICAL_SURFACE('',#5884,0.0125);
#5028=CYLINDRICAL_SURFACE('',#5885,0.0125);
#5029=CYLINDRICAL_SURFACE('',#5886,0.0125);
#5030=CYLINDRICAL_SURFACE('',#5887,0.0125);
#5031=CYLINDRICAL_SURFACE('',#5888,0.0048);
#5032=CYLINDRICAL_SURFACE('',#5889,0.011374);
#5033=CYLINDRICAL_SURFACE('',#5890,0.0048);
#5034=CYLINDRICAL_SURFACE('',#5891,0.0048);
#5035=CYLINDRICAL_SURFACE('',#5892,0.011374);
#5036=CYLINDRICAL_SURFACE('',#5893,0.0048);
#5037=CYLINDRICAL_SURFACE('',#5894,0.0048);
#5038=CYLINDRICAL_SURFACE('',#5895,0.011374);
#5039=CYLINDRICAL_SURFACE('',#5896,0.0048);
#5040=CYLINDRICAL_SURFACE('',#5897,0.0048);
#5041=CYLINDRICAL_SURFACE('',#5898,0.011374);
#5042=CYLINDRICAL_SURFACE('',#5899,0.0048);
#5043=CYLINDRICAL_SURFACE('',#5900,0.0048);
#5044=CYLINDRICAL_SURFACE('',#5901,0.011374);
#5045=CYLINDRICAL_SURFACE('',#5902,0.0048);
#5046=CYLINDRICAL_SURFACE('',#5903,0.0048);
#5047=CYLINDRICAL_SURFACE('',#5904,0.011374);
#5048=CYLINDRICAL_SURFACE('',#5905,0.0048);
#5049=CYLINDRICAL_SURFACE('',#5906,0.0048);
#5050=CYLINDRICAL_SURFACE('',#5907,0.011374);
#5051=CYLINDRICAL_SURFACE('',#5908,0.0048);
#5052=CYLINDRICAL_SURFACE('',#5909,0.0048);
#5053=CYLINDRICAL_SURFACE('',#5910,0.011374);
#5054=CYLINDRICAL_SURFACE('',#5911,0.0048);
#5055=CYLINDRICAL_SURFACE('',#5912,0.0048);
#5056=CYLINDRICAL_SURFACE('',#5913,0.011374);
#5057=CYLINDRICAL_SURFACE('',#5914,0.0048);
#5058=CYLINDRICAL_SURFACE('',#5915,0.0048);
#5059=CYLINDRICAL_SURFACE('',#5916,0.011374);
#5060=CYLINDRICAL_SURFACE('',#5917,0.0048);
#5061=CYLINDRICAL_SURFACE('',#5918,0.0048);
#5062=CYLINDRICAL_SURFACE('',#5919,0.011374);
#5063=CYLINDRICAL_SURFACE('',#5920,0.0048);
#5064=CYLINDRICAL_SURFACE('',#5933,0.002);
#5065=CYLINDRICAL_SURFACE('',#5936,0.002);
#5066=CYLINDRICAL_SURFACE('',#5939,0.002);
#5067=CYLINDRICAL_SURFACE('',#5942,0.002);
#5068=CYLINDRICAL_SURFACE('',#5945,0.002);
#5069=CYLINDRICAL_SURFACE('',#5948,0.002);
#5070=CYLINDRICAL_SURFACE('',#5951,0.002);
#5071=CYLINDRICAL_SURFACE('',#5954,0.002);
#5072=CYLINDRICAL_SURFACE('',#5971,0.004);
#5073=CYLINDRICAL_SURFACE('',#5978,0.002);
#5074=CYLINDRICAL_SURFACE('',#5982,0.002);
#5075=CYLINDRICAL_SURFACE('',#5988,0.0015);
#5076=CYLINDRICAL_SURFACE('',#5992,0.0015);
#5077=CYLINDRICAL_SURFACE('',#5996,0.0015);
#5078=CYLINDRICAL_SURFACE('',#5998,0.00500637669063053);
#5079=CYLINDRICAL_SURFACE('',#6014,0.003);
#5080=CYLINDRICAL_SURFACE('',#6016,0.003);
#5081=CYLINDRICAL_SURFACE('',#6018,0.0025);
#5082=CYLINDRICAL_SURFACE('',#6022,0.002);
#5083=CYLINDRICAL_SURFACE('',#6023,0.0015);
#5084=CYLINDRICAL_SURFACE('',#6029,0.002);
#5085=CYLINDRICAL_SURFACE('',#6030,0.0015);
#5086=CYLINDRICAL_SURFACE('',#6037,0.0015);
#5087=CYLINDRICAL_SURFACE('',#6041,0.0015);
#5088=CYLINDRICAL_SURFACE('',#6044,0.0015);
#5089=CYLINDRICAL_SURFACE('',#6047,0.0015);
#5090=CYLINDRICAL_SURFACE('',#6050,0.0015);
#5091=CYLINDRICAL_SURFACE('',#6057,0.0015);
#5092=CYLINDRICAL_SURFACE('',#6069,0.059);
#5093=CYLINDRICAL_SURFACE('',#6070,0.00145132271222225);
#5094=CYLINDRICAL_SURFACE('',#6071,0.0016601861613766);
#5095=CYLINDRICAL_SURFACE('',#6072,0.00250000000000006);
#5096=CYLINDRICAL_SURFACE('',#6074,0.0015);
#5097=CYLINDRICAL_SURFACE('',#6077,0.0025);
#5098=CYLINDRICAL_SURFACE('',#6169,0.006);
#5099=CYLINDRICAL_SURFACE('',#6171,0.006);
#5100=CYLINDRICAL_SURFACE('',#6173,0.006);
#5101=CYLINDRICAL_SURFACE('',#6175,0.006);
#5102=CYLINDRICAL_SURFACE('',#6177,0.006);
#5103=CYLINDRICAL_SURFACE('',#6179,0.006);
#5104=CYLINDRICAL_SURFACE('',#6181,0.006);
#5105=CYLINDRICAL_SURFACE('',#6183,0.006);
#5106=CYLINDRICAL_SURFACE('',#6185,0.006);
#5107=CYLINDRICAL_SURFACE('',#6187,0.006);
#5108=CYLINDRICAL_SURFACE('',#6189,0.006);
#5109=CYLINDRICAL_SURFACE('',#6191,0.006);
#5110=CYLINDRICAL_SURFACE('',#6193,0.006);
#5111=CYLINDRICAL_SURFACE('',#6195,0.006);
#5112=CYLINDRICAL_SURFACE('',#6197,0.006);
#5113=CYLINDRICAL_SURFACE('',#6199,0.006);
#5114=CYLINDRICAL_SURFACE('',#6201,0.006);
#5115=CYLINDRICAL_SURFACE('',#6203,0.006);
#5116=CYLINDRICAL_SURFACE('',#6205,0.006);
#5117=CYLINDRICAL_SURFACE('',#6207,0.006);
#5118=CYLINDRICAL_SURFACE('',#6209,0.006);
#5119=CYLINDRICAL_SURFACE('',#6279,0.006);
#5120=CYLINDRICAL_SURFACE('',#6280,0.0022);
#5121=CYLINDRICAL_SURFACE('',#6281,0.0022);
#5122=CYLINDRICAL_SURFACE('',#6282,0.004874);
#5123=CYLINDRICAL_SURFACE('',#6283,0.0022);
#5124=CYLINDRICAL_SURFACE('',#6284,0.0022);
#5125=CYLINDRICAL_SURFACE('',#6285,0.004874);
#5126=CYLINDRICAL_SURFACE('',#6286,0.0022);
#5127=CYLINDRICAL_SURFACE('',#6287,0.0022);
#5128=CYLINDRICAL_SURFACE('',#6288,0.004874);
#5129=CYLINDRICAL_SURFACE('',#6289,0.0022);
#5130=CYLINDRICAL_SURFACE('',#6290,0.0022);
#5131=CYLINDRICAL_SURFACE('',#6291,0.004874);
#5132=CYLINDRICAL_SURFACE('',#6292,0.0022);
#5133=CYLINDRICAL_SURFACE('',#6293,0.0022);
#5134=CYLINDRICAL_SURFACE('',#6294,0.004874);
#5135=CYLINDRICAL_SURFACE('',#6295,0.0022);
#5136=CYLINDRICAL_SURFACE('',#6296,0.0022);
#5137=CYLINDRICAL_SURFACE('',#6297,0.004874);
#5138=CYLINDRICAL_SURFACE('',#6298,0.0022);
#5139=CYLINDRICAL_SURFACE('',#6299,0.0022);
#5140=CYLINDRICAL_SURFACE('',#6300,0.004874);
#5141=CYLINDRICAL_SURFACE('',#6301,0.0022);
#5142=CYLINDRICAL_SURFACE('',#6302,0.0022);
#5143=CYLINDRICAL_SURFACE('',#6303,0.004874);
#5144=CYLINDRICAL_SURFACE('',#6304,0.0022);
#5145=CYLINDRICAL_SURFACE('',#6305,0.0022);
#5146=CYLINDRICAL_SURFACE('',#6306,0.004874);
#5147=CYLINDRICAL_SURFACE('',#6307,0.0022);
#5148=CYLINDRICAL_SURFACE('',#6308,0.0022);
#5149=CYLINDRICAL_SURFACE('',#6309,0.004874);
#5150=CYLINDRICAL_SURFACE('',#6310,0.0022);
#5151=CYLINDRICAL_SURFACE('',#6311,0.0022);
#5152=CYLINDRICAL_SURFACE('',#6312,0.004874);
#5153=CYLINDRICAL_SURFACE('',#6313,0.0022);
#5154=CYLINDRICAL_SURFACE('',#6314,0.0022);
#5155=CYLINDRICAL_SURFACE('',#6315,0.004874);
#5156=CYLINDRICAL_SURFACE('',#6316,0.0022);
#5157=CYLINDRICAL_SURFACE('',#6317,0.0022);
#5158=CYLINDRICAL_SURFACE('',#6318,0.004874);
#5159=CYLINDRICAL_SURFACE('',#6319,0.0022);
#5160=CYLINDRICAL_SURFACE('',#6320,0.0022);
#5161=CYLINDRICAL_SURFACE('',#6321,0.004874);
#5162=CYLINDRICAL_SURFACE('',#6322,0.0022);
#5163=CYLINDRICAL_SURFACE('',#6323,0.0022);
#5164=CYLINDRICAL_SURFACE('',#6324,0.004874);
#5165=CYLINDRICAL_SURFACE('',#6325,0.0022);
#5166=CYLINDRICAL_SURFACE('',#6326,0.0022);
#5167=CYLINDRICAL_SURFACE('',#6327,0.004874);
#5168=CYLINDRICAL_SURFACE('',#6328,0.0022);
#5169=CYLINDRICAL_SURFACE('',#6329,0.0022);
#5170=CYLINDRICAL_SURFACE('',#6330,0.004874);
#5171=CYLINDRICAL_SURFACE('',#6331,0.0022);
#5172=CYLINDRICAL_SURFACE('',#6332,0.0022);
#5173=CYLINDRICAL_SURFACE('',#6333,0.004874);
#5174=CYLINDRICAL_SURFACE('',#6334,0.0022);
#5175=CYLINDRICAL_SURFACE('',#6335,0.0022);
#5176=CYLINDRICAL_SURFACE('',#6336,0.004874);
#5177=CYLINDRICAL_SURFACE('',#6337,0.0022);
#5178=CYLINDRICAL_SURFACE('',#6338,0.0022);
#5179=CYLINDRICAL_SURFACE('',#6339,0.004874);
#5180=CYLINDRICAL_SURFACE('',#6340,0.0022);
#5181=CYLINDRICAL_SURFACE('',#6341,0.0022);
#5182=CYLINDRICAL_SURFACE('',#6342,0.004874);
#5183=CYLINDRICAL_SURFACE('',#6343,0.0022);
#5184=CYLINDRICAL_SURFACE('',#6344,0.0022);
#5185=CYLINDRICAL_SURFACE('',#6345,0.004874);
#5186=CYLINDRICAL_SURFACE('',#6351,0.00375738138352587);
#5187=CYLINDRICAL_SURFACE('',#6353,0.0015);
#5188=CYLINDRICAL_SURFACE('',#6358,0.0025);
#5189=CYLINDRICAL_SURFACE('',#6361,0.051);
#5190=CYLINDRICAL_SURFACE('',#6364,0.002);
#5191=CYLINDRICAL_SURFACE('',#6367,0.049);
#5192=CYLINDRICAL_SURFACE('',#6375,0.0015);
#5193=CYLINDRICAL_SURFACE('',#6381,0.0485);
#5194=CYLINDRICAL_SURFACE('',#6386,0.0515);
#5195=CYLINDRICAL_SURFACE('',#6394,0.0475);
#5196=CYLINDRICAL_SURFACE('',#6398,0.0525);
#5197=CYLINDRICAL_SURFACE('',#6411,0.002);
#5198=CYLINDRICAL_SURFACE('',#6413,0.002);
#5199=CYLINDRICAL_SURFACE('',#6415,0.0015);
#5200=CYLINDRICAL_SURFACE('',#6416,0.0015);
#5201=CYLINDRICAL_SURFACE('',#6418,0.0635);
#5202=CYLINDRICAL_SURFACE('',#6423,0.06);
#5203=CYLINDRICAL_SURFACE('',#6429,0.0645);
#5204=CYLINDRICAL_SURFACE('',#6435,0.0619081467766146);
#5205=CYLINDRICAL_SURFACE('',#6467,0.000257682665739803);
#5206=CYLINDRICAL_SURFACE('',#6468,0.00755256285496241);
#5207=CYLINDRICAL_SURFACE('',#6470,0.0025);
#5208=CYLINDRICAL_SURFACE('',#6473,0.0025);
#5209=CYLINDRICAL_SURFACE('',#6475,0.00755256285496241);
#5210=CYLINDRICAL_SURFACE('',#6476,0.000257682665739803);
#5211=CYLINDRICAL_SURFACE('',#6478,0.0015);
#5212=CYLINDRICAL_SURFACE('',#6485,0.00125);
#5213=ADVANCED_FACE('',(#4555,#4556,#4557),#5003,.F.);
#5214=ADVANCED_FACE('',(#4558,#4559,#4560),#5004,.T.);
#5215=ADVANCED_FACE('',(#4561,#4562),#699,.T.);
#5216=ADVANCED_FACE('',(#4563,#4564,#4565,#4566,#4567),#700,.F.);
#5217=ADVANCED_FACE('',(#4568,#4569),#5005,.T.);
#5218=ADVANCED_FACE('',(#4570,#4571),#701,.F.);
#5219=ADVANCED_FACE('',(#4572,#4573,#4574,#4575,#4576),#702,.F.);
#5220=ADVANCED_FACE('',(#4577,#4578),#5006,.F.);
#5221=ADVANCED_FACE('',(#4579,#4580),#5007,.F.);
#5222=ADVANCED_FACE('',(#4581,#4582),#5008,.F.);
#5223=ADVANCED_FACE('',(#4583,#4584),#5009,.F.);
#5224=ADVANCED_FACE('',(#4585,#4586),#5010,.F.);
#5225=ADVANCED_FACE('',(#4587),#703,.F.);
#5226=ADVANCED_FACE('',(#4588),#17,.T.);
#5227=ADVANCED_FACE('',(#4589,#4590),#5011,.T.);
#5228=ADVANCED_FACE('',(#4591),#704,.F.);
#5229=ADVANCED_FACE('',(#4592),#705,.F.);
#5230=ADVANCED_FACE('',(#4593,#4594),#10,.T.);
#5231=ADVANCED_FACE('',(#4595,#4596),#706,.F.);
#5232=ADVANCED_FACE('',(#4597,#4598),#18,.F.);
#5233=ADVANCED_FACE('',(#4599),#19,.T.);
#5234=ADVANCED_FACE('',(#4600),#707,.T.);
#5235=ADVANCED_FACE('',(#4601),#708,.F.);
#5236=ADVANCED_FACE('',(#4602),#709,.T.);
#5237=ADVANCED_FACE('',(#4603,#4604),#11,.T.);
#5238=ADVANCED_FACE('',(#4605),#5012,.T.);
#5239=ADVANCED_FACE('',(#4606),#5013,.T.);
#5240=ADVANCED_FACE('',(#4607,#4608),#5014,.F.);
#5241=ADVANCED_FACE('',(#4609,#4610,#4611),#710,.T.);
#5242=ADVANCED_FACE('',(#4612,#4613,#4614),#711,.F.);
#5243=ADVANCED_FACE('',(#4615),#712,.F.);
#5244=ADVANCED_FACE('',(#4616),#5015,.F.);
#5245=ADVANCED_FACE('',(#4617),#5016,.F.);
#5246=ADVANCED_FACE('',(#4618),#713,.F.);
#5247=ADVANCED_FACE('',(#4619),#5017,.T.);
#5248=ADVANCED_FACE('',(#4620),#714,.F.);
#5249=ADVANCED_FACE('',(#4621),#5018,.T.);
#5250=ADVANCED_FACE('',(#4622),#5019,.F.);
#5251=ADVANCED_FACE('',(#4623),#715,.T.);
#5252=ADVANCED_FACE('',(#4624),#5020,.F.);
#5253=ADVANCED_FACE('',(#4625),#716,.T.);
#5254=ADVANCED_FACE('',(#4626),#5021,.T.);
#5255=ADVANCED_FACE('',(#4627),#5022,.T.);
#5256=ADVANCED_FACE('',(#4628),#5023,.T.);
#5257=ADVANCED_FACE('',(#4629),#5024,.T.);
#5258=ADVANCED_FACE('',(#4630),#5025,.T.);
#5259=ADVANCED_FACE('',(#4631),#5026,.T.);
#5260=ADVANCED_FACE('',(#4632),#5027,.T.);
#5261=ADVANCED_FACE('',(#4633),#5028,.T.);
#5262=ADVANCED_FACE('',(#4634),#5029,.T.);
#5263=ADVANCED_FACE('',(#4635),#5030,.T.);
#5264=ADVANCED_FACE('',(#4636),#5031,.T.);
#5265=ADVANCED_FACE('',(#4637),#5032,.T.);
#5266=ADVANCED_FACE('',(#4638),#5033,.T.);
#5267=ADVANCED_FACE('',(#4639),#5034,.T.);
#5268=ADVANCED_FACE('',(#4640),#5035,.T.);
#5269=ADVANCED_FACE('',(#4641),#5036,.T.);
#5270=ADVANCED_FACE('',(#4642),#5037,.T.);
#5271=ADVANCED_FACE('',(#4643),#5038,.T.);
#5272=ADVANCED_FACE('',(#4644),#5039,.T.);
#5273=ADVANCED_FACE('',(#4645),#5040,.T.);
#5274=ADVANCED_FACE('',(#4646),#5041,.T.);
#5275=ADVANCED_FACE('',(#4647),#5042,.T.);
#5276=ADVANCED_FACE('',(#4648),#5043,.T.);
#5277=ADVANCED_FACE('',(#4649),#5044,.T.);
#5278=ADVANCED_FACE('',(#4650),#5045,.T.);
#5279=ADVANCED_FACE('',(#4651),#5046,.T.);
#5280=ADVANCED_FACE('',(#4652),#5047,.T.);
#5281=ADVANCED_FACE('',(#4653),#5048,.T.);
#5282=ADVANCED_FACE('',(#4654),#5049,.T.);
#5283=ADVANCED_FACE('',(#4655),#5050,.T.);
#5284=ADVANCED_FACE('',(#4656),#5051,.T.);
#5285=ADVANCED_FACE('',(#4657),#5052,.T.);
#5286=ADVANCED_FACE('',(#4658),#5053,.T.);
#5287=ADVANCED_FACE('',(#4659),#5054,.T.);
#5288=ADVANCED_FACE('',(#4660),#5055,.T.);
#5289=ADVANCED_FACE('',(#4661),#5056,.T.);
#5290=ADVANCED_FACE('',(#4662),#5057,.T.);
#5291=ADVANCED_FACE('',(#4663),#5058,.T.);
#5292=ADVANCED_FACE('',(#4664),#5059,.T.);
#5293=ADVANCED_FACE('',(#4665),#5060,.T.);
#5294=ADVANCED_FACE('',(#4666),#5061,.T.);
#5295=ADVANCED_FACE('',(#4667),#5062,.T.);
#5296=ADVANCED_FACE('',(#4668),#5063,.T.);
#5297=ADVANCED_FACE('',(#4669),#717,.T.);
#5298=ADVANCED_FACE('',(#4670),#718,.T.);
#5299=ADVANCED_FACE('',(#4671),#719,.F.);
#5300=ADVANCED_FACE('',(#4672),#720,.F.);
#5301=ADVANCED_FACE('',(#4673),#721,.F.);
#5302=ADVANCED_FACE('',(#4674),#722,.F.);
#5303=ADVANCED_FACE('',(#4675),#723,.T.);
#5304=ADVANCED_FACE('',(#4676),#724,.T.);
#5305=ADVANCED_FACE('',(#4677),#5064,.T.);
#5306=ADVANCED_FACE('',(#4678),#5065,.T.);
#5307=ADVANCED_FACE('',(#4679),#5066,.T.);
#5308=ADVANCED_FACE('',(#4680),#5067,.T.);
#5309=ADVANCED_FACE('',(#4681),#5068,.T.);
#5310=ADVANCED_FACE('',(#4682),#5069,.T.);
#5311=ADVANCED_FACE('',(#4683),#5070,.T.);
#5312=ADVANCED_FACE('',(#4684),#5071,.T.);
#5313=ADVANCED_FACE('',(#4685),#725,.F.);
#5314=ADVANCED_FACE('',(#4686),#726,.F.);
#5315=ADVANCED_FACE('',(#4687),#727,.F.);
#5316=ADVANCED_FACE('',(#4688),#728,.F.);
#5317=ADVANCED_FACE('',(#4689),#729,.F.);
#5318=ADVANCED_FACE('',(#4690),#730,.F.);
#5319=ADVANCED_FACE('',(#4691),#731,.T.);
#5320=ADVANCED_FACE('',(#4692,#4693),#5072,.T.);
#5321=ADVANCED_FACE('',(#4694,#4695),#732,.T.);
#5322=ADVANCED_FACE('',(#4696,#4697),#12,.T.);
#5323=ADVANCED_FACE('',(#4698),#5073,.F.);
#5324=ADVANCED_FACE('',(#4699),#733,.F.);
#5325=ADVANCED_FACE('',(#4700),#5074,.F.);
#5326=ADVANCED_FACE('',(#4701),#734,.F.);
#5327=ADVANCED_FACE('',(#4702),#735,.T.);
#5328=ADVANCED_FACE('',(#4703),#5075,.F.);
#5329=ADVANCED_FACE('',(#4704),#736,.F.);
#5330=ADVANCED_FACE('',(#4705),#5076,.F.);
#5331=ADVANCED_FACE('',(#4706),#737,.F.);
#5332=ADVANCED_FACE('',(#4707),#738,.T.);
#5333=ADVANCED_FACE('',(#4708,#4709),#5077,.F.);
#5334=ADVANCED_FACE('',(#4710,#4711),#20,.F.);
#5335=ADVANCED_FACE('',(#4712,#4713),#5078,.T.);
#5336=ADVANCED_FACE('',(#4714,#4715),#739,.T.);
#5337=ADVANCED_FACE('',(#4716,#4717),#740,.T.);
#5338=ADVANCED_FACE('',(#4718,#4719,#4720,#4721),#741,.T.);
#5339=ADVANCED_FACE('',(#4722,#4723),#742,.F.);
#5340=ADVANCED_FACE('',(#4724),#5079,.T.);
#5341=ADVANCED_FACE('',(#4725),#743,.F.);
#5342=ADVANCED_FACE('',(#4726),#5080,.T.);
#5343=ADVANCED_FACE('',(#4727),#744,.F.);
#5344=ADVANCED_FACE('',(#4728,#4729),#5081,.F.);
#5345=ADVANCED_FACE('',(#4730,#4731),#745,.T.);
#5346=ADVANCED_FACE('',(#4732,#4733),#5082,.T.);
#5347=ADVANCED_FACE('',(#4734,#4735),#5083,.F.);
#5348=ADVANCED_FACE('',(#4736),#746,.T.);
#5349=ADVANCED_FACE('',(#4737,#4738),#747,.T.);
#5350=ADVANCED_FACE('',(#4739,#4740),#5084,.T.);
#5351=ADVANCED_FACE('',(#4741,#4742),#5085,.F.);
#5352=ADVANCED_FACE('',(#4743),#748,.T.);
#5353=ADVANCED_FACE('',(#4744),#749,.T.);
#5354=ADVANCED_FACE('',(#4745),#750,.F.);
#5355=ADVANCED_FACE('',(#4746),#751,.F.);
#5356=ADVANCED_FACE('',(#4747,#4748),#5086,.F.);
#5357=ADVANCED_FACE('',(#4749),#752,.T.);
#5358=ADVANCED_FACE('',(#4750,#4751),#5087,.F.);
#5359=ADVANCED_FACE('',(#4752,#4753),#5088,.F.);
#5360=ADVANCED_FACE('',(#4754,#4755),#5089,.F.);
#5361=ADVANCED_FACE('',(#4756,#4757),#5090,.F.);
#5362=ADVANCED_FACE('',(#4758,#4759,#4760,#4761,#4762,#4763,#4764),#753,
 .F.);
#5363=ADVANCED_FACE('',(#4765,#4766,#4767,#4768,#4769,#4770,#4771),#754,
 .T.);
#5364=ADVANCED_FACE('',(#4772,#4773),#5091,.F.);
#5365=ADVANCED_FACE('',(#4774,#4775,#4776,#4777),#755,.T.);
#5366=ADVANCED_FACE('',(#4778,#4779,#4780,#4781),#756,.F.);
#5367=ADVANCED_FACE('',(#4782,#4783),#5092,.T.);
#5368=ADVANCED_FACE('',(#4784,#4785),#5093,.F.);
#5369=ADVANCED_FACE('',(#4786,#4787),#5094,.F.);
#5370=ADVANCED_FACE('',(#4788,#4789),#5095,.F.);
#5371=ADVANCED_FACE('',(#4790,#4791),#5096,.F.);
#5372=ADVANCED_FACE('',(#4792,#4793),#5097,.T.);
#5373=ADVANCED_FACE('',(#4794,#4795),#757,.F.);
#5374=ADVANCED_FACE('',(#4796),#5098,.T.);
#5375=ADVANCED_FACE('',(#4797),#5099,.T.);
#5376=ADVANCED_FACE('',(#4798),#5100,.T.);
#5377=ADVANCED_FACE('',(#4799),#5101,.T.);
#5378=ADVANCED_FACE('',(#4800),#5102,.T.);
#5379=ADVANCED_FACE('',(#4801),#5103,.T.);
#5380=ADVANCED_FACE('',(#4802),#5104,.T.);
#5381=ADVANCED_FACE('',(#4803),#5105,.T.);
#5382=ADVANCED_FACE('',(#4804),#5106,.T.);
#5383=ADVANCED_FACE('',(#4805),#5107,.T.);
#5384=ADVANCED_FACE('',(#4806),#5108,.T.);
#5385=ADVANCED_FACE('',(#4807),#5109,.T.);
#5386=ADVANCED_FACE('',(#4808),#5110,.T.);
#5387=ADVANCED_FACE('',(#4809),#5111,.T.);
#5388=ADVANCED_FACE('',(#4810),#5112,.T.);
#5389=ADVANCED_FACE('',(#4811),#5113,.T.);
#5390=ADVANCED_FACE('',(#4812),#5114,.T.);
#5391=ADVANCED_FACE('',(#4813),#5115,.T.);
#5392=ADVANCED_FACE('',(#4814),#5116,.T.);
#5393=ADVANCED_FACE('',(#4815),#5117,.T.);
#5394=ADVANCED_FACE('',(#4816),#5118,.T.);
#5395=ADVANCED_FACE('',(#4817,#4818),#758,.F.);
#5396=ADVANCED_FACE('',(#4819),#5119,.T.);
#5397=ADVANCED_FACE('',(#4820),#5120,.T.);
#5398=ADVANCED_FACE('',(#4821),#5121,.T.);
#5399=ADVANCED_FACE('',(#4822),#5122,.T.);
#5400=ADVANCED_FACE('',(#4823),#5123,.T.);
#5401=ADVANCED_FACE('',(#4824),#5124,.T.);
#5402=ADVANCED_FACE('',(#4825),#5125,.T.);
#5403=ADVANCED_FACE('',(#4826),#5126,.T.);
#5404=ADVANCED_FACE('',(#4827),#5127,.T.);
#5405=ADVANCED_FACE('',(#4828),#5128,.T.);
#5406=ADVANCED_FACE('',(#4829),#5129,.T.);
#5407=ADVANCED_FACE('',(#4830),#5130,.T.);
#5408=ADVANCED_FACE('',(#4831),#5131,.T.);
#5409=ADVANCED_FACE('',(#4832),#5132,.T.);
#5410=ADVANCED_FACE('',(#4833),#5133,.T.);
#5411=ADVANCED_FACE('',(#4834),#5134,.T.);
#5412=ADVANCED_FACE('',(#4835),#5135,.T.);
#5413=ADVANCED_FACE('',(#4836),#5136,.T.);
#5414=ADVANCED_FACE('',(#4837),#5137,.T.);
#5415=ADVANCED_FACE('',(#4838),#5138,.T.);
#5416=ADVANCED_FACE('',(#4839),#5139,.T.);
#5417=ADVANCED_FACE('',(#4840),#5140,.T.);
#5418=ADVANCED_FACE('',(#4841),#5141,.T.);
#5419=ADVANCED_FACE('',(#4842),#5142,.T.);
#5420=ADVANCED_FACE('',(#4843),#5143,.T.);
#5421=ADVANCED_FACE('',(#4844),#5144,.T.);
#5422=ADVANCED_FACE('',(#4845),#5145,.T.);
#5423=ADVANCED_FACE('',(#4846),#5146,.T.);
#5424=ADVANCED_FACE('',(#4847),#5147,.T.);
#5425=ADVANCED_FACE('',(#4848),#5148,.T.);
#5426=ADVANCED_FACE('',(#4849),#5149,.T.);
#5427=ADVANCED_FACE('',(#4850),#5150,.T.);
#5428=ADVANCED_FACE('',(#4851),#5151,.T.);
#5429=ADVANCED_FACE('',(#4852),#5152,.T.);
#5430=ADVANCED_FACE('',(#4853),#5153,.T.);
#5431=ADVANCED_FACE('',(#4854),#5154,.T.);
#5432=ADVANCED_FACE('',(#4855),#5155,.T.);
#5433=ADVANCED_FACE('',(#4856),#5156,.T.);
#5434=ADVANCED_FACE('',(#4857),#5157,.T.);
#5435=ADVANCED_FACE('',(#4858),#5158,.T.);
#5436=ADVANCED_FACE('',(#4859),#5159,.T.);
#5437=ADVANCED_FACE('',(#4860),#5160,.T.);
#5438=ADVANCED_FACE('',(#4861),#5161,.T.);
#5439=ADVANCED_FACE('',(#4862),#5162,.T.);
#5440=ADVANCED_FACE('',(#4863),#5163,.T.);
#5441=ADVANCED_FACE('',(#4864),#5164,.T.);
#5442=ADVANCED_FACE('',(#4865),#5165,.T.);
#5443=ADVANCED_FACE('',(#4866),#5166,.T.);
#5444=ADVANCED_FACE('',(#4867),#5167,.T.);
#5445=ADVANCED_FACE('',(#4868),#5168,.T.);
#5446=ADVANCED_FACE('',(#4869),#5169,.T.);
#5447=ADVANCED_FACE('',(#4870),#5170,.T.);
#5448=ADVANCED_FACE('',(#4871),#5171,.T.);
#5449=ADVANCED_FACE('',(#4872),#5172,.T.);
#5450=ADVANCED_FACE('',(#4873),#5173,.T.);
#5451=ADVANCED_FACE('',(#4874),#5174,.T.);
#5452=ADVANCED_FACE('',(#4875),#5175,.T.);
#5453=ADVANCED_FACE('',(#4876),#5176,.T.);
#5454=ADVANCED_FACE('',(#4877),#5177,.T.);
#5455=ADVANCED_FACE('',(#4878),#5178,.T.);
#5456=ADVANCED_FACE('',(#4879),#5179,.T.);
#5457=ADVANCED_FACE('',(#4880),#5180,.T.);
#5458=ADVANCED_FACE('',(#4881),#5181,.T.);
#5459=ADVANCED_FACE('',(#4882),#5182,.T.);
#5460=ADVANCED_FACE('',(#4883),#5183,.T.);
#5461=ADVANCED_FACE('',(#4884),#5184,.T.);
#5462=ADVANCED_FACE('',(#4885),#5185,.T.);
#5463=ADVANCED_FACE('',(#4886,#4887),#759,.T.);
#5464=ADVANCED_FACE('',(#4888,#4889),#760,.F.);
#5465=ADVANCED_FACE('',(#4890,#4891),#5186,.T.);
#5466=ADVANCED_FACE('',(#4892),#761,.F.);
#5467=ADVANCED_FACE('',(#4893,#4894),#5187,.F.);
#5468=ADVANCED_FACE('',(#4895,#4896),#762,.T.);
#5469=ADVANCED_FACE('',(#4897,#4898),#5188,.T.);
#5470=ADVANCED_FACE('',(#4899),#763,.T.);
#5471=ADVANCED_FACE('',(#4900),#5189,.T.);
#5472=ADVANCED_FACE('',(#4901),#5190,.T.);
#5473=ADVANCED_FACE('',(#4902),#5191,.F.);
#5474=ADVANCED_FACE('',(#4903),#764,.T.);
#5475=ADVANCED_FACE('',(#4904,#4905),#765,.F.);
#5476=ADVANCED_FACE('',(#4906,#4907),#766,.T.);
#5477=ADVANCED_FACE('',(#4908,#4909),#5192,.F.);
#5478=ADVANCED_FACE('',(#4910),#21,.F.);
#5479=ADVANCED_FACE('',(#4911),#5193,.T.);
#5480=ADVANCED_FACE('',(#4912),#22,.F.);
#5481=ADVANCED_FACE('',(#4913),#5194,.F.);
#5482=ADVANCED_FACE('',(#4914,#4915),#767,.F.);
#5483=ADVANCED_FACE('',(#4916,#4917),#768,.F.);
#5484=ADVANCED_FACE('',(#4918),#23,.T.);
#5485=ADVANCED_FACE('',(#4919),#5195,.F.);
#5486=ADVANCED_FACE('',(#4920),#24,.T.);
#5487=ADVANCED_FACE('',(#4921),#5196,.T.);
#5488=ADVANCED_FACE('',(#4922,#4923,#4924),#769,.T.);
#5489=ADVANCED_FACE('',(#4925,#4926,#4927),#770,.F.);
#5490=ADVANCED_FACE('',(#4928),#5197,.T.);
#5491=ADVANCED_FACE('',(#4929),#771,.F.);
#5492=ADVANCED_FACE('',(#4930),#5198,.T.);
#5493=ADVANCED_FACE('',(#4931),#772,.F.);
#5494=ADVANCED_FACE('',(#4932,#4933),#5199,.F.);
#5495=ADVANCED_FACE('',(#4934,#4935),#5200,.F.);
#5496=ADVANCED_FACE('',(#4936,#4937),#5201,.F.);
#5497=ADVANCED_FACE('',(#4938,#4939),#773,.F.);
#5498=ADVANCED_FACE('',(#4940,#4941),#5202,.F.);
#5499=ADVANCED_FACE('',(#4942,#4943),#13,.F.);
#5500=ADVANCED_FACE('',(#4944,#4945),#14,.T.);
#5501=ADVANCED_FACE('',(#4946,#4947),#5203,.T.);
#5502=ADVANCED_FACE('',(#4948,#4949),#774,.F.);
#5503=ADVANCED_FACE('',(#4950,#4951),#5204,.F.);
#5504=ADVANCED_FACE('',(#4952,#4953),#775,.F.);
#5505=ADVANCED_FACE('',(#4954,#4955),#25,.T.);
#5506=ADVANCED_FACE('',(#4956,#4957),#26,.T.);
#5507=ADVANCED_FACE('',(#4958,#4959),#27,.F.);
#5508=ADVANCED_FACE('',(#4960,#4961),#28,.F.);
#5509=ADVANCED_FACE('',(#4962,#4963),#29,.T.);
#5510=ADVANCED_FACE('',(#4964,#4965),#30,.T.);
#5511=ADVANCED_FACE('',(#4966,#4967),#31,.T.);
#5512=ADVANCED_FACE('',(#4968,#4969),#776,.T.);
#5513=ADVANCED_FACE('',(#4970,#4971),#777,.F.);
#5514=ADVANCED_FACE('',(#4972),#5205,.T.);
#5515=ADVANCED_FACE('',(#4973),#5206,.F.);
#5516=ADVANCED_FACE('',(#4974),#778,.F.);
#5517=ADVANCED_FACE('',(#4975),#5207,.T.);
#5518=ADVANCED_FACE('',(#4976),#779,.F.);
#5519=ADVANCED_FACE('',(#4977),#780,.F.);
#5520=ADVANCED_FACE('',(#4978),#5208,.T.);
#5521=ADVANCED_FACE('',(#4979),#781,.F.);
#5522=ADVANCED_FACE('',(#4980),#5209,.F.);
#5523=ADVANCED_FACE('',(#4981),#5210,.T.);
#5524=ADVANCED_FACE('',(#4982),#782,.F.);
#5525=ADVANCED_FACE('',(#4983,#4984),#5211,.F.);
#5526=ADVANCED_FACE('',(#4985),#783,.F.);
#5527=ADVANCED_FACE('',(#4986),#32,.T.);
#5528=ADVANCED_FACE('',(#4987,#4988),#5212,.T.);
#5529=ADVANCED_FACE('',(#4989),#784,.F.);
#5530=ADVANCED_FACE('',(#4990),#785,.F.);
#5531=ADVANCED_FACE('',(#4991,#4992),#15,.T.);
#5532=ADVANCED_FACE('',(#4993,#4994),#786,.F.);
#5533=ADVANCED_FACE('',(#4995,#4996),#33,.F.);
#5534=ADVANCED_FACE('',(#4997),#34,.T.);
#5535=ADVANCED_FACE('',(#4998),#787,.T.);
#5536=ADVANCED_FACE('',(#4999),#788,.F.);
#5537=ADVANCED_FACE('',(#5000),#789,.T.);
#5538=ADVANCED_FACE('',(#5001,#5002),#16,.T.);
#5539=CLOSED_SHELL('',(#5213,#5214,#5215,#5216,#5217,#5218,#5219,#5220,
#5221,#5222,#5223,#5224));
#5540=CLOSED_SHELL('',(#5225,#5226,#5227,#5228,#5229,#5230,#5231,#5232,
#5233,#5234,#5235,#5236,#5237));
#5541=CLOSED_SHELL('',(#5238,#5239,#5240,#5241,#5242,#5243,#5244,#5245,
#5246,#5247,#5248,#5249,#5250,#5251,#5252,#5253,#5254,#5255,#5256,#5257,
#5258,#5259,#5260,#5261,#5262,#5263,#5264,#5265,#5266,#5267,#5268,#5269,
#5270,#5271,#5272,#5273,#5274,#5275,#5276,#5277,#5278,#5279,#5280,#5281,
#5282,#5283,#5284,#5285,#5286,#5287,#5288,#5289,#5290,#5291,#5292,#5293,
#5294,#5295,#5296));
#5542=CLOSED_SHELL('',(#5297,#5298,#5299,#5300,#5301,#5302,#5303,#5304,
#5305,#5306,#5307,#5308,#5309,#5310,#5311,#5312,#5313,#5314,#5315,#5316,
#5317,#5318,#5319,#5320,#5321,#5322,#5323,#5324,#5325,#5326,#5327,#5328,
#5329,#5330,#5331,#5332,#5333,#5334,#5335,#5336,#5337));
#5543=CLOSED_SHELL('',(#5338,#5339,#5340,#5341,#5342,#5343,#5344,#5345,
#5346,#5347,#5348,#5349,#5350,#5351,#5352));
#5544=CLOSED_SHELL('',(#5353,#5354,#5355,#5356,#5357,#5358,#5359,#5360,
#5361,#5362,#5363,#5364));
#5545=CLOSED_SHELL('',(#5365,#5366,#5367,#5368,#5369,#5370));
#5546=CLOSED_SHELL('',(#5371,#5372,#5373,#5374,#5375,#5376,#5377,#5378,
#5379,#5380,#5381,#5382,#5383,#5384,#5385,#5386,#5387,#5388,#5389,#5390,
#5391,#5392,#5393,#5394,#5395,#5396,#5397,#5398,#5399,#5400,#5401,#5402,
#5403,#5404,#5405,#5406,#5407,#5408,#5409,#5410,#5411,#5412,#5413,#5414,
#5415,#5416,#5417,#5418,#5419,#5420,#5421,#5422,#5423,#5424,#5425,#5426,
#5427,#5428,#5429,#5430,#5431,#5432,#5433,#5434,#5435,#5436,#5437,#5438,
#5439,#5440,#5441,#5442,#5443,#5444,#5445,#5446,#5447,#5448,#5449,#5450,
#5451,#5452,#5453,#5454,#5455,#5456,#5457,#5458,#5459,#5460,#5461,#5462,
#5463,#5464,#5465,#5466,#5467,#5468,#5469,#5470));
#5547=CLOSED_SHELL('',(#5471,#5472,#5473,#5474,#5475,#5476,#5477));
#5548=CLOSED_SHELL('',(#5478,#5479,#5480,#5481,#5482,#5483,#5484,#5485,
#5486,#5487));
#5549=CLOSED_SHELL('',(#5488,#5489,#5490,#5491,#5492,#5493,#5494,#5495));
#5550=CLOSED_SHELL('',(#5496,#5497,#5498,#5499,#5500,#5501,#5502,#5503,
#5504,#5505,#5506,#5507,#5508,#5509,#5510,#5511));
#5551=CLOSED_SHELL('',(#5512,#5513,#5514,#5515,#5516,#5517,#5518,#5519,
#5520,#5521,#5522,#5523,#5524,#5525));
#5552=CLOSED_SHELL('',(#5526,#5527,#5528,#5529,#5530,#5531,#5532,#5533,
#5534,#5535,#5536,#5537,#5538));
#5553=STYLED_ITEM('',(#5567),#5658);
#5554=STYLED_ITEM('',(#5568),#5659);
#5555=STYLED_ITEM('',(#5569),#5660);
#5556=STYLED_ITEM('',(#5570),#5661);
#5557=STYLED_ITEM('',(#5571),#5662);
#5558=STYLED_ITEM('',(#5572),#5663);
#5559=STYLED_ITEM('',(#5573),#5664);
#5560=STYLED_ITEM('',(#5574),#5665);
#5561=STYLED_ITEM('',(#5575),#5666);
#5562=STYLED_ITEM('',(#5576),#5667);
#5563=STYLED_ITEM('',(#5577),#5668);
#5564=STYLED_ITEM('',(#5578),#5669);
#5565=STYLED_ITEM('',(#5579),#5670);
#5566=STYLED_ITEM('',(#5580),#5671);
#5567=PRESENTATION_STYLE_ASSIGNMENT((#5581));
#5568=PRESENTATION_STYLE_ASSIGNMENT((#5582));
#5569=PRESENTATION_STYLE_ASSIGNMENT((#5583));
#5570=PRESENTATION_STYLE_ASSIGNMENT((#5584));
#5571=PRESENTATION_STYLE_ASSIGNMENT((#5585));
#5572=PRESENTATION_STYLE_ASSIGNMENT((#5586));
#5573=PRESENTATION_STYLE_ASSIGNMENT((#5587));
#5574=PRESENTATION_STYLE_ASSIGNMENT((#5588));
#5575=PRESENTATION_STYLE_ASSIGNMENT((#5589));
#5576=PRESENTATION_STYLE_ASSIGNMENT((#5590));
#5577=PRESENTATION_STYLE_ASSIGNMENT((#5591));
#5578=PRESENTATION_STYLE_ASSIGNMENT((#5592));
#5579=PRESENTATION_STYLE_ASSIGNMENT((#5593));
#5580=PRESENTATION_STYLE_ASSIGNMENT((#5594));
#5581=SURFACE_STYLE_USAGE(.BOTH.,#5595);
#5582=SURFACE_STYLE_USAGE(.BOTH.,#5596);
#5583=SURFACE_STYLE_USAGE(.BOTH.,#5597);
#5584=SURFACE_STYLE_USAGE(.BOTH.,#5598);
#5585=SURFACE_STYLE_USAGE(.BOTH.,#5599);
#5586=SURFACE_STYLE_USAGE(.BOTH.,#5600);
#5587=SURFACE_STYLE_USAGE(.BOTH.,#5601);
#5588=SURFACE_STYLE_USAGE(.BOTH.,#5602);
#5589=SURFACE_STYLE_USAGE(.BOTH.,#5603);
#5590=SURFACE_STYLE_USAGE(.BOTH.,#5604);
#5591=SURFACE_STYLE_USAGE(.BOTH.,#5605);
#5592=SURFACE_STYLE_USAGE(.BOTH.,#5606);
#5593=SURFACE_STYLE_USAGE(.BOTH.,#5607);
#5594=SURFACE_STYLE_USAGE(.BOTH.,#5608);
#5595=SURFACE_SIDE_STYLE('',(#5609));
#5596=SURFACE_SIDE_STYLE('',(#5610));
#5597=SURFACE_SIDE_STYLE('',(#5611));
#5598=SURFACE_SIDE_STYLE('',(#5612));
#5599=SURFACE_SIDE_STYLE('',(#5613));
#5600=SURFACE_SIDE_STYLE('',(#5614));
#5601=SURFACE_SIDE_STYLE('',(#5615));
#5602=SURFACE_SIDE_STYLE('',(#5616));
#5603=SURFACE_SIDE_STYLE('',(#5617));
#5604=SURFACE_SIDE_STYLE('',(#5618));
#5605=SURFACE_SIDE_STYLE('',(#5619));
#5606=SURFACE_SIDE_STYLE('',(#5620));
#5607=SURFACE_SIDE_STYLE('',(#5621));
#5608=SURFACE_SIDE_STYLE('',(#5622));
#5609=SURFACE_STYLE_FILL_AREA(#5623);
#5610=SURFACE_STYLE_FILL_AREA(#5624);
#5611=SURFACE_STYLE_FILL_AREA(#5625);
#5612=SURFACE_STYLE_FILL_AREA(#5626);
#5613=SURFACE_STYLE_FILL_AREA(#5627);
#5614=SURFACE_STYLE_FILL_AREA(#5628);
#5615=SURFACE_STYLE_FILL_AREA(#5629);
#5616=SURFACE_STYLE_FILL_AREA(#5630);
#5617=SURFACE_STYLE_FILL_AREA(#5631);
#5618=SURFACE_STYLE_FILL_AREA(#5632);
#5619=SURFACE_STYLE_FILL_AREA(#5633);
#5620=SURFACE_STYLE_FILL_AREA(#5634);
#5621=SURFACE_STYLE_FILL_AREA(#5635);
#5622=SURFACE_STYLE_FILL_AREA(#5636);
#5623=FILL_AREA_STYLE('',(#5637));
#5624=FILL_AREA_STYLE('',(#5638));
#5625=FILL_AREA_STYLE('',(#5639));
#5626=FILL_AREA_STYLE('',(#5640));
#5627=FILL_AREA_STYLE('',(#5641));
#5628=FILL_AREA_STYLE('',(#5642));
#5629=FILL_AREA_STYLE('',(#5643));
#5630=FILL_AREA_STYLE('',(#5644));
#5631=FILL_AREA_STYLE('',(#5645));
#5632=FILL_AREA_STYLE('',(#5646));
#5633=FILL_AREA_STYLE('',(#5647));
#5634=FILL_AREA_STYLE('',(#5648));
#5635=FILL_AREA_STYLE('',(#5649));
#5636=FILL_AREA_STYLE('',(#5650));
#5637=FILL_AREA_STYLE_COLOUR('',#5651);
#5638=FILL_AREA_STYLE_COLOUR('',#5652);
#5639=FILL_AREA_STYLE_COLOUR('',#5653);
#5640=FILL_AREA_STYLE_COLOUR('',#5654);
#5641=FILL_AREA_STYLE_COLOUR('',#5653);
#5642=FILL_AREA_STYLE_COLOUR('',#5653);
#5643=FILL_AREA_STYLE_COLOUR('',#5653);
#5644=FILL_AREA_STYLE_COLOUR('',#5655);
#5645=FILL_AREA_STYLE_COLOUR('',#5656);
#5646=FILL_AREA_STYLE_COLOUR('',#5656);
#5647=FILL_AREA_STYLE_COLOUR('',#5653);
#5648=FILL_AREA_STYLE_COLOUR('',#5651);
#5649=FILL_AREA_STYLE_COLOUR('',#5657);
#5650=FILL_AREA_STYLE_COLOUR('',#5652);
#5651=COLOUR_RGB('', 0.66274510, 0.83137255, 0.94901961);
#5652=COLOUR_RGB('', 0.31764706, 0.68627451, 0.89019608);
#5653=COLOUR_RGB('', 0.40784314, 0.44705882, 0.49803922);
#5654=COLOUR_RGB('', 0.72549020, 0.75294118, 0.79215686);
#5655=COLOUR_RGB('', 0.31764706, 0.68627451, 0.89019608);
#5656=COLOUR_RGB('', 0.40784314, 0.44705882, 0.49803922);
#5657=COLOUR_RGB('', 0.66274510, 0.83137255, 0.94901961);
#5658=MANIFOLD_SOLID_BREP('Part 1',#5539);
#5659=MANIFOLD_SOLID_BREP('Slotted cheese head screw M2.5x0.45 x 10',#5540);
#5660=MANIFOLD_SOLID_BREP('Part 1',#5541);
#5661=MANIFOLD_SOLID_BREP('Part 1',#5542);
#5662=MANIFOLD_SOLID_BREP('Part 3',#5543);
#5663=MANIFOLD_SOLID_BREP('Part 2',#5544);
#5664=MANIFOLD_SOLID_BREP('Part 1',#5545);
#5665=MANIFOLD_SOLID_BREP('Part 1',#5546);
#5666=MANIFOLD_SOLID_BREP('Part 2',#5547);
#5667=MANIFOLD_SOLID_BREP('Part 3',#5548);
#5668=MANIFOLD_SOLID_BREP('Part 1',#5549);
#5669=MANIFOLD_SOLID_BREP('Part 1',#5550);
#5670=MANIFOLD_SOLID_BREP('Part 1',#5551);
#5671=MANIFOLD_SOLID_BREP('Slotted cheese head screw M2.5x0.45 x 6',#5552);
#5672=SHAPE_DEFINITION_REPRESENTATION(#10177,#5688);
#5673=SHAPE_DEFINITION_REPRESENTATION(#10178,#5689);
#5674=SHAPE_DEFINITION_REPRESENTATION(#10180,#5690);
#5675=SHAPE_DEFINITION_REPRESENTATION(#10183,#5691);
#5676=SHAPE_DEFINITION_REPRESENTATION(#10186,#5692);
#5677=SHAPE_DEFINITION_REPRESENTATION(#10188,#5693);
#5678=SHAPE_DEFINITION_REPRESENTATION(#10190,#5694);
#5679=SHAPE_DEFINITION_REPRESENTATION(#10192,#5695);
#5680=SHAPE_DEFINITION_REPRESENTATION(#10194,#5696);
#5681=SHAPE_DEFINITION_REPRESENTATION(#10196,#5697);
#5682=SHAPE_DEFINITION_REPRESENTATION(#10197,#5698);
#5683=SHAPE_DEFINITION_REPRESENTATION(#10199,#5699);
#5684=SHAPE_DEFINITION_REPRESENTATION(#10202,#5700);
#5685=SHAPE_DEFINITION_REPRESENTATION(#10204,#5701);
#5686=SHAPE_DEFINITION_REPRESENTATION(#10206,#5702);
#5687=SHAPE_DEFINITION_REPRESENTATION(#10208,#5703);
#5688=SHAPE_REPRESENTATION('MAS-674',(#5704,#5731,#5756,#5757,#5921,
#5922,#6003,#6033,#6058,#6073,#6360,#6400,#6417,#6450,#6479,#6504),#10142);
#5689=SHAPE_REPRESENTATION('Part 1',(#5704),#10143);
#5690=SHAPE_REPRESENTATION('Slotted cheese head screw M2.5x0.45 x 10',(#5704),
#10144);
#5691=SHAPE_REPRESENTATION('Part 1',(#5704),#10145);
#5692=SHAPE_REPRESENTATION('Part 1',(#5704),#10146);
#5693=SHAPE_REPRESENTATION('Part 3',(#5704),#10147);
#5694=SHAPE_REPRESENTATION('Part 2',(#5704),#10148);
#5695=SHAPE_REPRESENTATION('Part 1',(#5704),#10149);
#5696=SHAPE_REPRESENTATION('Part 1',(#5704),#10150);
#5697=SHAPE_REPRESENTATION('Assembly 2 <1>',(#5704,#6376,#6399),#10151);
#5698=SHAPE_REPRESENTATION('Part 2',(#5704),#10152);
#5699=SHAPE_REPRESENTATION('Part 3',(#5704),#10153);
#5700=SHAPE_REPRESENTATION('Part 1',(#5704),#10154);
#5701=SHAPE_REPRESENTATION('Part 1',(#5704),#10155);
#5702=SHAPE_REPRESENTATION('Part 1',(#5704),#10156);
#5703=SHAPE_REPRESENTATION('Slotted cheese head screw M2.5x0.45 x 6',(#5704),
#10157);
#5704=AXIS2_PLACEMENT_3D('',#8391,#6505,#6506);
#5705=AXIS2_PLACEMENT_3D('',#8392,#6507,#6508);
#5706=AXIS2_PLACEMENT_3D('',#8393,#6509,#6510);
#5707=AXIS2_PLACEMENT_3D('',#8395,#6511,#6512);
#5708=AXIS2_PLACEMENT_3D('',#8409,#6513,#6514);
#5709=AXIS2_PLACEMENT_3D('',#8410,#6515,#6516);
#5710=AXIS2_PLACEMENT_3D('',#8412,#6517,#6518);
#5711=AXIS2_PLACEMENT_3D('',#8426,#6519,#6520);
#5712=AXIS2_PLACEMENT_3D('',#8427,#6521,#6522);
#5713=AXIS2_PLACEMENT_3D('',#8429,#6523,#6524);
#5714=AXIS2_PLACEMENT_3D('',#8430,#6525,#6526);
#5715=AXIS2_PLACEMENT_3D('',#8432,#6527,#6528);
#5716=AXIS2_PLACEMENT_3D('',#8434,#6529,#6530);
#5717=AXIS2_PLACEMENT_3D('',#8436,#6531,#6532);
#5718=AXIS2_PLACEMENT_3D('',#8438,#6533,#6534);
#5719=AXIS2_PLACEMENT_3D('',#8439,#6535,#6536);
#5720=AXIS2_PLACEMENT_3D('',#8441,#6537,#6538);
#5721=AXIS2_PLACEMENT_3D('',#8442,#6539,#6540);
#5722=AXIS2_PLACEMENT_3D('',#8443,#6541,#6542);
#5723=AXIS2_PLACEMENT_3D('',#8445,#6543,#6544);
#5724=AXIS2_PLACEMENT_3D('',#8447,#6545,#6546);
#5725=AXIS2_PLACEMENT_3D('',#8449,#6547,#6548);
#5726=AXIS2_PLACEMENT_3D('',#8451,#6549,#6550);
#5727=AXIS2_PLACEMENT_3D('',#8452,#6551,#6552);
#5728=AXIS2_PLACEMENT_3D('',#8453,#6553,#6554);
#5729=AXIS2_PLACEMENT_3D('',#8454,#6555,#6556);
#5730=AXIS2_PLACEMENT_3D('',#8455,#6557,#6558);
#5731=AXIS2_PLACEMENT_3D('',#8456,#6559,#6560);
#5732=AXIS2_PLACEMENT_3D('',#8457,#6561,#6562);
#5733=AXIS2_PLACEMENT_3D('',#8461,#6564,#6565);
#5734=AXIS2_PLACEMENT_3D('',#8462,#6566,#6567);
#5735=AXIS2_PLACEMENT_3D('',#8463,#6568,#6569);
#5736=AXIS2_PLACEMENT_3D('',#8471,#6570,#6571);
#5737=AXIS2_PLACEMENT_3D('',#8477,#6572,#6573);
#5738=AXIS2_PLACEMENT_3D('',#8478,#6574,#6575);
#5739=AXIS2_PLACEMENT_3D('',#8480,#6576,#6577);
#5740=AXIS2_PLACEMENT_3D('',#8482,#6578,#6579);
#5741=AXIS2_PLACEMENT_3D('',#8483,#6580,#6581);
#5742=AXIS2_PLACEMENT_3D('',#8485,#6582,#6583);
#5743=AXIS2_PLACEMENT_3D('',#8487,#6585,#6586);
#5744=AXIS2_PLACEMENT_3D('',#8488,#6587,#6588);
#5745=AXIS2_PLACEMENT_3D('',#8496,#6589,#6590);
#5746=AXIS2_PLACEMENT_3D('',#8507,#6591,#6592);
#5747=AXIS2_PLACEMENT_3D('',#8513,#6593,#6594);
#5748=AXIS2_PLACEMENT_3D('',#8515,#6595,#6596);
#5749=AXIS2_PLACEMENT_3D('',#8516,#6597,#6598);
#5750=AXIS2_PLACEMENT_3D('',#8518,#6599,#6600);
#5751=AXIS2_PLACEMENT_3D('',#8519,#6601,#6602);
#5752=AXIS2_PLACEMENT_3D('',#8528,#6603,#6604);
#5753=AXIS2_PLACEMENT_3D('',#8531,#6607,#6608);
#5754=AXIS2_PLACEMENT_3D('',#8532,#6609,#6610);
#5755=AXIS2_PLACEMENT_3D('',#8533,#6611,#6612);
#5756=AXIS2_PLACEMENT_3D('',#8534,#6613,#6614);
#5757=AXIS2_PLACEMENT_3D('',#8535,#6615,#6616);
#5758=AXIS2_PLACEMENT_3D('',#8536,#6617,#6618);
#5759=AXIS2_PLACEMENT_3D('',#8537,#6619,#6620);
#5760=AXIS2_PLACEMENT_3D('',#8542,#6622,#6623);
#5761=AXIS2_PLACEMENT_3D('',#8545,#6625,#6626);
#5762=AXIS2_PLACEMENT_3D('',#8546,#6627,#6628);
#5763=AXIS2_PLACEMENT_3D('',#8551,#6630,#6631);
#5764=AXIS2_PLACEMENT_3D('',#8554,#6633,#6634);
#5765=AXIS2_PLACEMENT_3D('',#8555,#6635,#6636);
#5766=AXIS2_PLACEMENT_3D('',#8557,#6637,#6638);
#5767=AXIS2_PLACEMENT_3D('',#8559,#6639,#6640);
#5768=AXIS2_PLACEMENT_3D('',#8563,#6642,#6643);
#5769=AXIS2_PLACEMENT_3D('',#8567,#6645,#6646);
#5770=AXIS2_PLACEMENT_3D('',#8568,#6647,#6648);
#5771=AXIS2_PLACEMENT_3D('',#8570,#6649,#6650);
#5772=AXIS2_PLACEMENT_3D('',#8572,#6651,#6652);
#5773=AXIS2_PLACEMENT_3D('',#8574,#6653,#6654);
#5774=AXIS2_PLACEMENT_3D('',#8576,#6655,#6656);
#5775=AXIS2_PLACEMENT_3D('',#8578,#6657,#6658);
#5776=AXIS2_PLACEMENT_3D('',#8580,#6659,#6660);
#5777=AXIS2_PLACEMENT_3D('',#8582,#6661,#6662);
#5778=AXIS2_PLACEMENT_3D('',#8584,#6663,#6664);
#5779=AXIS2_PLACEMENT_3D('',#8586,#6665,#6666);
#5780=AXIS2_PLACEMENT_3D('',#8588,#6667,#6668);
#5781=AXIS2_PLACEMENT_3D('',#8590,#6669,#6670);
#5782=AXIS2_PLACEMENT_3D('',#8592,#6671,#6672);
#5783=AXIS2_PLACEMENT_3D('',#8594,#6673,#6674);
#5784=AXIS2_PLACEMENT_3D('',#8596,#6675,#6676);
#5785=AXIS2_PLACEMENT_3D('',#8598,#6677,#6678);
#5786=AXIS2_PLACEMENT_3D('',#8600,#6679,#6680);
#5787=AXIS2_PLACEMENT_3D('',#8602,#6681,#6682);
#5788=AXIS2_PLACEMENT_3D('',#8604,#6683,#6684);
#5789=AXIS2_PLACEMENT_3D('',#8606,#6685,#6686);
#5790=AXIS2_PLACEMENT_3D('',#8608,#6687,#6688);
#5791=AXIS2_PLACEMENT_3D('',#8610,#6689,#6690);
#5792=AXIS2_PLACEMENT_3D('',#8612,#6691,#6692);
#5793=AXIS2_PLACEMENT_3D('',#8614,#6693,#6694);
#5794=AXIS2_PLACEMENT_3D('',#8616,#6695,#6696);
#5795=AXIS2_PLACEMENT_3D('',#8618,#6697,#6698);
#5796=AXIS2_PLACEMENT_3D('',#8620,#6699,#6700);
#5797=AXIS2_PLACEMENT_3D('',#8622,#6701,#6702);
#5798=AXIS2_PLACEMENT_3D('',#8624,#6703,#6704);
#5799=AXIS2_PLACEMENT_3D('',#8626,#6705,#6706);
#5800=AXIS2_PLACEMENT_3D('',#8628,#6707,#6708);
#5801=AXIS2_PLACEMENT_3D('',#8630,#6709,#6710);
#5802=AXIS2_PLACEMENT_3D('',#8632,#6711,#6712);
#5803=AXIS2_PLACEMENT_3D('',#8634,#6713,#6714);
#5804=AXIS2_PLACEMENT_3D('',#8636,#6715,#6716);
#5805=AXIS2_PLACEMENT_3D('',#8638,#6717,#6718);
#5806=AXIS2_PLACEMENT_3D('',#8640,#6719,#6720);
#5807=AXIS2_PLACEMENT_3D('',#8642,#6721,#6722);
#5808=AXIS2_PLACEMENT_3D('',#8644,#6723,#6724);
#5809=AXIS2_PLACEMENT_3D('',#8646,#6725,#6726);
#5810=AXIS2_PLACEMENT_3D('',#8648,#6727,#6728);
#5811=AXIS2_PLACEMENT_3D('',#8650,#6729,#6730);
#5812=AXIS2_PLACEMENT_3D('',#8652,#6731,#6732);
#5813=AXIS2_PLACEMENT_3D('',#8655,#6734,#6735);
#5814=AXIS2_PLACEMENT_3D('',#8659,#6737,#6738);
#5815=AXIS2_PLACEMENT_3D('',#8663,#6740,#6741);
#5816=AXIS2_PLACEMENT_3D('',#8665,#6742,#6743);
#5817=AXIS2_PLACEMENT_3D('',#8666,#6744,#6745);
#5818=AXIS2_PLACEMENT_3D('',#8667,#6746,#6747);
#5819=AXIS2_PLACEMENT_3D('',#8669,#6748,#6749);
#5820=AXIS2_PLACEMENT_3D('',#8671,#6750,#6751);
#5821=AXIS2_PLACEMENT_3D('',#8675,#6753,#6754);
#5822=AXIS2_PLACEMENT_3D('',#8679,#6756,#6757);
#5823=AXIS2_PLACEMENT_3D('',#8682,#6759,#6760);
#5824=AXIS2_PLACEMENT_3D('',#8684,#6761,#6762);
#5825=AXIS2_PLACEMENT_3D('',#8686,#6763,#6764);
#5826=AXIS2_PLACEMENT_3D('',#8688,#6765,#6766);
#5827=AXIS2_PLACEMENT_3D('',#8690,#6767,#6768);
#5828=AXIS2_PLACEMENT_3D('',#8692,#6769,#6770);
#5829=AXIS2_PLACEMENT_3D('',#8694,#6771,#6772);
#5830=AXIS2_PLACEMENT_3D('',#8696,#6773,#6774);
#5831=AXIS2_PLACEMENT_3D('',#8698,#6775,#6776);
#5832=AXIS2_PLACEMENT_3D('',#8700,#6777,#6778);
#5833=AXIS2_PLACEMENT_3D('',#8702,#6779,#6780);
#5834=AXIS2_PLACEMENT_3D('',#8704,#6781,#6782);
#5835=AXIS2_PLACEMENT_3D('',#8706,#6783,#6784);
#5836=AXIS2_PLACEMENT_3D('',#8708,#6785,#6786);
#5837=AXIS2_PLACEMENT_3D('',#8710,#6787,#6788);
#5838=AXIS2_PLACEMENT_3D('',#8712,#6789,#6790);
#5839=AXIS2_PLACEMENT_3D('',#8714,#6791,#6792);
#5840=AXIS2_PLACEMENT_3D('',#8716,#6793,#6794);
#5841=AXIS2_PLACEMENT_3D('',#8718,#6795,#6796);
#5842=AXIS2_PLACEMENT_3D('',#8720,#6797,#6798);
#5843=AXIS2_PLACEMENT_3D('',#8722,#6799,#6800);
#5844=AXIS2_PLACEMENT_3D('',#8724,#6801,#6802);
#5845=AXIS2_PLACEMENT_3D('',#8726,#6803,#6804);
#5846=AXIS2_PLACEMENT_3D('',#8728,#6805,#6806);
#5847=AXIS2_PLACEMENT_3D('',#8730,#6807,#6808);
#5848=AXIS2_PLACEMENT_3D('',#8732,#6809,#6810);
#5849=AXIS2_PLACEMENT_3D('',#8734,#6811,#6812);
#5850=AXIS2_PLACEMENT_3D('',#8736,#6813,#6814);
#5851=AXIS2_PLACEMENT_3D('',#8738,#6815,#6816);
#5852=AXIS2_PLACEMENT_3D('',#8740,#6817,#6818);
#5853=AXIS2_PLACEMENT_3D('',#8742,#6819,#6820);
#5854=AXIS2_PLACEMENT_3D('',#8744,#6821,#6822);
#5855=AXIS2_PLACEMENT_3D('',#8746,#6823,#6824);
#5856=AXIS2_PLACEMENT_3D('',#8748,#6825,#6826);
#5857=AXIS2_PLACEMENT_3D('',#8750,#6827,#6828);
#5858=AXIS2_PLACEMENT_3D('',#8752,#6829,#6830);
#5859=AXIS2_PLACEMENT_3D('',#8754,#6831,#6832);
#5860=AXIS2_PLACEMENT_3D('',#8756,#6833,#6834);
#5861=AXIS2_PLACEMENT_3D('',#8758,#6835,#6836);
#5862=AXIS2_PLACEMENT_3D('',#8760,#6837,#6838);
#5863=AXIS2_PLACEMENT_3D('',#8762,#6839,#6840);
#5864=AXIS2_PLACEMENT_3D('',#8764,#6841,#6842);
#5865=AXIS2_PLACEMENT_3D('',#8765,#6843,#6844);
#5866=AXIS2_PLACEMENT_3D('',#8770,#6846,#6847);
#5867=AXIS2_PLACEMENT_3D('',#8773,#6849,#6850);
#5868=AXIS2_PLACEMENT_3D('',#8775,#6852,#6853);
#5869=AXIS2_PLACEMENT_3D('',#8777,#6855,#6856);
#5870=AXIS2_PLACEMENT_3D('',#8779,#6858,#6859);
#5871=AXIS2_PLACEMENT_3D('',#8781,#6861,#6862);
#5872=AXIS2_PLACEMENT_3D('',#8783,#6864,#6865);
#5873=AXIS2_PLACEMENT_3D('',#8785,#6867,#6868);
#5874=AXIS2_PLACEMENT_3D('',#8786,#6869,#6870);
#5875=AXIS2_PLACEMENT_3D('',#8789,#6873,#6874);
#5876=AXIS2_PLACEMENT_3D('',#8791,#6876,#6877);
#5877=AXIS2_PLACEMENT_3D('',#8793,#6879,#6880);
#5878=AXIS2_PLACEMENT_3D('',#8794,#6881,#6882);
#5879=AXIS2_PLACEMENT_3D('',#8797,#6885,#6886);
#5880=AXIS2_PLACEMENT_3D('',#8800,#6889,#6890);
#5881=AXIS2_PLACEMENT_3D('',#8803,#6893,#6894);
#5882=AXIS2_PLACEMENT_3D('',#8806,#6897,#6898);
#5883=AXIS2_PLACEMENT_3D('',#8809,#6901,#6902);
#5884=AXIS2_PLACEMENT_3D('',#8812,#6905,#6906);
#5885=AXIS2_PLACEMENT_3D('',#8815,#6909,#6910);
#5886=AXIS2_PLACEMENT_3D('',#8818,#6913,#6914);
#5887=AXIS2_PLACEMENT_3D('',#8821,#6917,#6918);
#5888=AXIS2_PLACEMENT_3D('',#8824,#6921,#6922);
#5889=AXIS2_PLACEMENT_3D('',#8826,#6924,#6925);
#5890=AXIS2_PLACEMENT_3D('',#8828,#6927,#6928);
#5891=AXIS2_PLACEMENT_3D('',#8829,#6929,#6930);
#5892=AXIS2_PLACEMENT_3D('',#8831,#6932,#6933);
#5893=AXIS2_PLACEMENT_3D('',#8833,#6935,#6936);
#5894=AXIS2_PLACEMENT_3D('',#8834,#6937,#6938);
#5895=AXIS2_PLACEMENT_3D('',#8836,#6940,#6941);
#5896=AXIS2_PLACEMENT_3D('',#8838,#6943,#6944);
#5897=AXIS2_PLACEMENT_3D('',#8839,#6945,#6946);
#5898=AXIS2_PLACEMENT_3D('',#8841,#6948,#6949);
#5899=AXIS2_PLACEMENT_3D('',#8843,#6951,#6952);
#5900=AXIS2_PLACEMENT_3D('',#8844,#6953,#6954);
#5901=AXIS2_PLACEMENT_3D('',#8846,#6956,#6957);
#5902=AXIS2_PLACEMENT_3D('',#8848,#6959,#6960);
#5903=AXIS2_PLACEMENT_3D('',#8849,#6961,#6962);
#5904=AXIS2_PLACEMENT_3D('',#8851,#6964,#6965);
#5905=AXIS2_PLACEMENT_3D('',#8853,#6967,#6968);
#5906=AXIS2_PLACEMENT_3D('',#8854,#6969,#6970);
#5907=AXIS2_PLACEMENT_3D('',#8856,#6972,#6973);
#5908=AXIS2_PLACEMENT_3D('',#8858,#6975,#6976);
#5909=AXIS2_PLACEMENT_3D('',#8859,#6977,#6978);
#5910=AXIS2_PLACEMENT_3D('',#8861,#6980,#6981);
#5911=AXIS2_PLACEMENT_3D('',#8863,#6983,#6984);
#5912=AXIS2_PLACEMENT_3D('',#8864,#6985,#6986);
#5913=AXIS2_PLACEMENT_3D('',#8866,#6988,#6989);
#5914=AXIS2_PLACEMENT_3D('',#8868,#6991,#6992);
#5915=AXIS2_PLACEMENT_3D('',#8869,#6993,#6994);
#5916=AXIS2_PLACEMENT_3D('',#8871,#6996,#6997);
#5917=AXIS2_PLACEMENT_3D('',#8873,#6999,#7000);
#5918=AXIS2_PLACEMENT_3D('',#8874,#7001,#7002);
#5919=AXIS2_PLACEMENT_3D('',#8876,#7004,#7005);
#5920=AXIS2_PLACEMENT_3D('',#8878,#7007,#7008);
#5921=AXIS2_PLACEMENT_3D('',#8879,#7009,#7010);
#5922=AXIS2_PLACEMENT_3D('',#8880,#7011,#7012);
#5923=AXIS2_PLACEMENT_3D('',#8881,#7013,#7014);
#5924=AXIS2_PLACEMENT_3D('',#8890,#7019,#7020);
#5925=AXIS2_PLACEMENT_3D('',#8901,#7026,#7027);
#5926=AXIS2_PLACEMENT_3D('',#8907,#7030,#7031);
#5927=AXIS2_PLACEMENT_3D('',#8911,#7033,#7034);
#5928=AXIS2_PLACEMENT_3D('',#8914,#7036,#7037);
#5929=AXIS2_PLACEMENT_3D('',#8925,#7043,#7044);
#5930=AXIS2_PLACEMENT_3D('',#8934,#7049,#7050);
#5931=AXIS2_PLACEMENT_3D('',#8945,#7056,#7057);
#5932=AXIS2_PLACEMENT_3D('',#8954,#7062,#7063);
#5933=AXIS2_PLACEMENT_3D('',#8965,#7069,#7070);
#5934=AXIS2_PLACEMENT_3D('',#8966,#7071,#7072);
#5935=AXIS2_PLACEMENT_3D('',#8967,#7073,#7074);
#5936=AXIS2_PLACEMENT_3D('',#8976,#7076,#7077);
#5937=AXIS2_PLACEMENT_3D('',#8977,#7078,#7079);
#5938=AXIS2_PLACEMENT_3D('',#8978,#7080,#7081);
#5939=AXIS2_PLACEMENT_3D('',#8979,#7082,#7083);
#5940=AXIS2_PLACEMENT_3D('',#8980,#7084,#7085);
#5941=AXIS2_PLACEMENT_3D('',#8981,#7086,#7087);
#5942=AXIS2_PLACEMENT_3D('',#8982,#7088,#7089);
#5943=AXIS2_PLACEMENT_3D('',#8983,#7090,#7091);
#5944=AXIS2_PLACEMENT_3D('',#8984,#7092,#7093);
#5945=AXIS2_PLACEMENT_3D('',#8985,#7094,#7095);
#5946=AXIS2_PLACEMENT_3D('',#8986,#7096,#7097);
#5947=AXIS2_PLACEMENT_3D('',#8987,#7098,#7099);
#5948=AXIS2_PLACEMENT_3D('',#8988,#7100,#7101);
#5949=AXIS2_PLACEMENT_3D('',#8989,#7102,#7103);
#5950=AXIS2_PLACEMENT_3D('',#8990,#7104,#7105);
#5951=AXIS2_PLACEMENT_3D('',#8991,#7106,#7107);
#5952=AXIS2_PLACEMENT_3D('',#8992,#7108,#7109);
#5953=AXIS2_PLACEMENT_3D('',#9001,#7111,#7112);
#5954=AXIS2_PLACEMENT_3D('',#9002,#7113,#7114);
#5955=AXIS2_PLACEMENT_3D('',#9003,#7115,#7116);
#5956=AXIS2_PLACEMENT_3D('',#9004,#7117,#7118);
#5957=AXIS2_PLACEMENT_3D('',#9005,#7119,#7120);
#5958=AXIS2_PLACEMENT_3D('',#9007,#7122,#7123);
#5959=AXIS2_PLACEMENT_3D('',#9011,#7125,#7126);
#5960=AXIS2_PLACEMENT_3D('',#9012,#7127,#7128);
#5961=AXIS2_PLACEMENT_3D('',#9013,#7129,#7130);
#5962=AXIS2_PLACEMENT_3D('',#9014,#7131,#7132);
#5963=AXIS2_PLACEMENT_3D('',#9015,#7133,#7134);
#5964=AXIS2_PLACEMENT_3D('',#9016,#7135,#7136);
#5965=AXIS2_PLACEMENT_3D('',#9017,#7137,#7138);
#5966=AXIS2_PLACEMENT_3D('',#9018,#7139,#7140);
#5967=AXIS2_PLACEMENT_3D('',#9022,#7142,#7143);
#5968=AXIS2_PLACEMENT_3D('',#9027,#7146,#7147);
#5969=AXIS2_PLACEMENT_3D('',#9028,#7148,#7149);
#5970=AXIS2_PLACEMENT_3D('',#9029,#7150,#7151);
#5971=AXIS2_PLACEMENT_3D('',#9030,#7152,#7153);
#5972=AXIS2_PLACEMENT_3D('',#9031,#7154,#7155);
#5973=AXIS2_PLACEMENT_3D('',#9033,#7156,#7157);
#5974=AXIS2_PLACEMENT_3D('',#9035,#7158,#7159);
#5975=AXIS2_PLACEMENT_3D('',#9036,#7160,#7161);
#5976=AXIS2_PLACEMENT_3D('',#9038,#7162,#7163);
#5977=AXIS2_PLACEMENT_3D('',#9040,#7164,#7165);
#5978=AXIS2_PLACEMENT_3D('',#9041,#7166,#7167);
#5979=AXIS2_PLACEMENT_3D('',#9044,#7169,#7170);
#5980=AXIS2_PLACEMENT_3D('',#9047,#7172,#7173);
#5981=AXIS2_PLACEMENT_3D('',#9050,#7175,#7176);
#5982=AXIS2_PLACEMENT_3D('',#9055,#7179,#7180);
#5983=AXIS2_PLACEMENT_3D('',#9056,#7181,#7182);
#5984=AXIS2_PLACEMENT_3D('',#9059,#7184,#7185);
#5985=AXIS2_PLACEMENT_3D('',#9061,#7187,#7188);
#5986=AXIS2_PLACEMENT_3D('',#9063,#7190,#7191);
#5987=AXIS2_PLACEMENT_3D('',#9067,#7193,#7194);
#5988=AXIS2_PLACEMENT_3D('',#9072,#7197,#7198);
#5989=AXIS2_PLACEMENT_3D('',#9075,#7200,#7201);
#5990=AXIS2_PLACEMENT_3D('',#9078,#7203,#7204);
#5991=AXIS2_PLACEMENT_3D('',#9080,#7206,#7207);
#5992=AXIS2_PLACEMENT_3D('',#9081,#7208,#7209);
#5993=AXIS2_PLACEMENT_3D('',#9082,#7210,#7211);
#5994=AXIS2_PLACEMENT_3D('',#9085,#7213,#7214);
#5995=AXIS2_PLACEMENT_3D('',#9087,#7216,#7217);
#5996=AXIS2_PLACEMENT_3D('',#9088,#7218,#7219);
#5997=AXIS2_PLACEMENT_3D('',#9089,#7220,#7221);
#5998=AXIS2_PLACEMENT_3D('',#9090,#7222,#7223);
#5999=AXIS2_PLACEMENT_3D('',#9091,#7224,#7225);
#6000=AXIS2_PLACEMENT_3D('',#9093,#7226,#7227);
#6001=AXIS2_PLACEMENT_3D('',#9095,#7228,#7229);
#6002=AXIS2_PLACEMENT_3D('',#9096,#7230,#7231);
#6003=AXIS2_PLACEMENT_3D('',#9097,#7232,#7233);
#6004=AXIS2_PLACEMENT_3D('',#9098,#7234,#7235);
#6005=AXIS2_PLACEMENT_3D('',#9099,#7236,#7237);
#6006=AXIS2_PLACEMENT_3D('',#9101,#7238,#7239);
#6007=AXIS2_PLACEMENT_3D('',#9103,#7240,#7241);
#6008=AXIS2_PLACEMENT_3D('',#9108,#7243,#7244);
#6009=AXIS2_PLACEMENT_3D('',#9111,#7246,#7247);
#6010=AXIS2_PLACEMENT_3D('',#9113,#7248,#7249);
#6011=AXIS2_PLACEMENT_3D('',#9114,#7250,#7251);
#6012=AXIS2_PLACEMENT_3D('',#9119,#7253,#7254);
#6013=AXIS2_PLACEMENT_3D('',#9122,#7256,#7257);
#6014=AXIS2_PLACEMENT_3D('',#9124,#7258,#7259);
#6015=AXIS2_PLACEMENT_3D('',#9127,#7262,#7263);
#6016=AXIS2_PLACEMENT_3D('',#9129,#7265,#7266);
#6017=AXIS2_PLACEMENT_3D('',#9131,#7268,#7269);
#6018=AXIS2_PLACEMENT_3D('',#9132,#7270,#7271);
#6019=AXIS2_PLACEMENT_3D('',#9133,#7272,#7273);
#6020=AXIS2_PLACEMENT_3D('',#9134,#7274,#7275);
#6021=AXIS2_PLACEMENT_3D('',#9136,#7276,#7277);
#6022=AXIS2_PLACEMENT_3D('',#9138,#7278,#7279);
#6023=AXIS2_PLACEMENT_3D('',#9139,#7280,#7281);
#6024=AXIS2_PLACEMENT_3D('',#9140,#7282,#7283);
#6025=AXIS2_PLACEMENT_3D('',#9142,#7284,#7285);
#6026=AXIS2_PLACEMENT_3D('',#9143,#7286,#7287);
#6027=AXIS2_PLACEMENT_3D('',#9144,#7288,#7289);
#6028=AXIS2_PLACEMENT_3D('',#9146,#7290,#7291);
#6029=AXIS2_PLACEMENT_3D('',#9148,#7292,#7293);
#6030=AXIS2_PLACEMENT_3D('',#9149,#7294,#7295);
#6031=AXIS2_PLACEMENT_3D('',#9150,#7296,#7297);
#6032=AXIS2_PLACEMENT_3D('',#9152,#7298,#7299);
#6033=AXIS2_PLACEMENT_3D('',#9153,#7300,#7301);
#6034=AXIS2_PLACEMENT_3D('',#9154,#7302,#7303);
#6035=AXIS2_PLACEMENT_3D('',#9163,#7308,#7309);
#6036=AXIS2_PLACEMENT_3D('',#9169,#7313,#7314);
#6037=AXIS2_PLACEMENT_3D('',#9175,#7318,#7319);
#6038=AXIS2_PLACEMENT_3D('',#9176,#7320,#7321);
#6039=AXIS2_PLACEMENT_3D('',#9178,#7322,#7323);
#6040=AXIS2_PLACEMENT_3D('',#9180,#7324,#7325);
#6041=AXIS2_PLACEMENT_3D('',#9183,#7328,#7329);
#6042=AXIS2_PLACEMENT_3D('',#9184,#7330,#7331);
#6043=AXIS2_PLACEMENT_3D('',#9186,#7332,#7333);
#6044=AXIS2_PLACEMENT_3D('',#9188,#7334,#7335);
#6045=AXIS2_PLACEMENT_3D('',#9189,#7336,#7337);
#6046=AXIS2_PLACEMENT_3D('',#9191,#7338,#7339);
#6047=AXIS2_PLACEMENT_3D('',#9193,#7340,#7341);
#6048=AXIS2_PLACEMENT_3D('',#9194,#7342,#7343);
#6049=AXIS2_PLACEMENT_3D('',#9196,#7344,#7345);
#6050=AXIS2_PLACEMENT_3D('',#9198,#7346,#7347);
#6051=AXIS2_PLACEMENT_3D('',#9199,#7348,#7349);
#6052=AXIS2_PLACEMENT_3D('',#9201,#7350,#7351);
#6053=AXIS2_PLACEMENT_3D('',#9203,#7352,#7353);
#6054=AXIS2_PLACEMENT_3D('',#9204,#7354,#7355);
#6055=AXIS2_PLACEMENT_3D('',#9206,#7356,#7357);
#6056=AXIS2_PLACEMENT_3D('',#9207,#7358,#7359);
#6057=AXIS2_PLACEMENT_3D('',#9209,#7360,#7361);
#6058=AXIS2_PLACEMENT_3D('',#9210,#7362,#7363);
#6059=AXIS2_PLACEMENT_3D('',#9211,#7364,#7365);
#6060=AXIS2_PLACEMENT_3D('',#9212,#7366,#7367);
#6061=AXIS2_PLACEMENT_3D('',#9214,#7368,#7369);
#6062=AXIS2_PLACEMENT_3D('',#9216,#7370,#7371);
#6063=AXIS2_PLACEMENT_3D('',#9218,#7372,#7373);
#6064=AXIS2_PLACEMENT_3D('',#9220,#7374,#7375);
#6065=AXIS2_PLACEMENT_3D('',#9221,#7376,#7377);
#6066=AXIS2_PLACEMENT_3D('',#9223,#7378,#7379);
#6067=AXIS2_PLACEMENT_3D('',#9225,#7380,#7381);
#6068=AXIS2_PLACEMENT_3D('',#9227,#7382,#7383);
#6069=AXIS2_PLACEMENT_3D('',#9229,#7384,#7385);
#6070=AXIS2_PLACEMENT_3D('',#9230,#7386,#7387);
#6071=AXIS2_PLACEMENT_3D('',#9231,#7388,#7389);
#6072=AXIS2_PLACEMENT_3D('',#9232,#7390,#7391);
#6073=AXIS2_PLACEMENT_3D('',#9233,#7392,#7393);
#6074=AXIS2_PLACEMENT_3D('',#9234,#7394,#7395);
#6075=AXIS2_PLACEMENT_3D('',#9235,#7396,#7397);
#6076=AXIS2_PLACEMENT_3D('',#9237,#7398,#7399);
#6077=AXIS2_PLACEMENT_3D('',#9239,#7400,#7401);
#6078=AXIS2_PLACEMENT_3D('',#9240,#7402,#7403);
#6079=AXIS2_PLACEMENT_3D('',#9242,#7404,#7405);
#6080=AXIS2_PLACEMENT_3D('',#9244,#7406,#7407);
#6081=AXIS2_PLACEMENT_3D('',#9245,#7408,#7409);
#6082=AXIS2_PLACEMENT_3D('',#9248,#7410,#7411);
#6083=AXIS2_PLACEMENT_3D('',#9250,#7412,#7413);
#6084=AXIS2_PLACEMENT_3D('',#9252,#7414,#7415);
#6085=AXIS2_PLACEMENT_3D('',#9254,#7416,#7417);
#6086=AXIS2_PLACEMENT_3D('',#9256,#7418,#7419);
#6087=AXIS2_PLACEMENT_3D('',#9258,#7420,#7421);
#6088=AXIS2_PLACEMENT_3D('',#9260,#7422,#7423);
#6089=AXIS2_PLACEMENT_3D('',#9262,#7424,#7425);
#6090=AXIS2_PLACEMENT_3D('',#9264,#7426,#7427);
#6091=AXIS2_PLACEMENT_3D('',#9266,#7428,#7429);
#6092=AXIS2_PLACEMENT_3D('',#9268,#7430,#7431);
#6093=AXIS2_PLACEMENT_3D('',#9270,#7432,#7433);
#6094=AXIS2_PLACEMENT_3D('',#9272,#7434,#7435);
#6095=AXIS2_PLACEMENT_3D('',#9274,#7436,#7437);
#6096=AXIS2_PLACEMENT_3D('',#9276,#7438,#7439);
#6097=AXIS2_PLACEMENT_3D('',#9278,#7440,#7441);
#6098=AXIS2_PLACEMENT_3D('',#9280,#7442,#7443);
#6099=AXIS2_PLACEMENT_3D('',#9282,#7444,#7445);
#6100=AXIS2_PLACEMENT_3D('',#9284,#7446,#7447);
#6101=AXIS2_PLACEMENT_3D('',#9286,#7448,#7449);
#6102=AXIS2_PLACEMENT_3D('',#9288,#7450,#7451);
#6103=AXIS2_PLACEMENT_3D('',#9290,#7452,#7453);
#6104=AXIS2_PLACEMENT_3D('',#9292,#7454,#7455);
#6105=AXIS2_PLACEMENT_3D('',#9294,#7456,#7457);
#6106=AXIS2_PLACEMENT_3D('',#9296,#7458,#7459);
#6107=AXIS2_PLACEMENT_3D('',#9298,#7460,#7461);
#6108=AXIS2_PLACEMENT_3D('',#9300,#7462,#7463);
#6109=AXIS2_PLACEMENT_3D('',#9302,#7464,#7465);
#6110=AXIS2_PLACEMENT_3D('',#9304,#7466,#7467);
#6111=AXIS2_PLACEMENT_3D('',#9306,#7468,#7469);
#6112=AXIS2_PLACEMENT_3D('',#9308,#7470,#7471);
#6113=AXIS2_PLACEMENT_3D('',#9310,#7472,#7473);
#6114=AXIS2_PLACEMENT_3D('',#9312,#7474,#7475);
#6115=AXIS2_PLACEMENT_3D('',#9314,#7476,#7477);
#6116=AXIS2_PLACEMENT_3D('',#9316,#7478,#7479);
#6117=AXIS2_PLACEMENT_3D('',#9318,#7480,#7481);
#6118=AXIS2_PLACEMENT_3D('',#9320,#7482,#7483);
#6119=AXIS2_PLACEMENT_3D('',#9322,#7484,#7485);
#6120=AXIS2_PLACEMENT_3D('',#9324,#7486,#7487);
#6121=AXIS2_PLACEMENT_3D('',#9326,#7488,#7489);
#6122=AXIS2_PLACEMENT_3D('',#9328,#7490,#7491);
#6123=AXIS2_PLACEMENT_3D('',#9330,#7492,#7493);
#6124=AXIS2_PLACEMENT_3D('',#9332,#7494,#7495);
#6125=AXIS2_PLACEMENT_3D('',#9334,#7496,#7497);
#6126=AXIS2_PLACEMENT_3D('',#9336,#7498,#7499);
#6127=AXIS2_PLACEMENT_3D('',#9338,#7500,#7501);
#6128=AXIS2_PLACEMENT_3D('',#9340,#7502,#7503);
#6129=AXIS2_PLACEMENT_3D('',#9342,#7504,#7505);
#6130=AXIS2_PLACEMENT_3D('',#9344,#7506,#7507);
#6131=AXIS2_PLACEMENT_3D('',#9346,#7508,#7509);
#6132=AXIS2_PLACEMENT_3D('',#9348,#7510,#7511);
#6133=AXIS2_PLACEMENT_3D('',#9350,#7512,#7513);
#6134=AXIS2_PLACEMENT_3D('',#9352,#7514,#7515);
#6135=AXIS2_PLACEMENT_3D('',#9354,#7516,#7517);
#6136=AXIS2_PLACEMENT_3D('',#9356,#7518,#7519);
#6137=AXIS2_PLACEMENT_3D('',#9358,#7520,#7521);
#6138=AXIS2_PLACEMENT_3D('',#9360,#7522,#7523);
#6139=AXIS2_PLACEMENT_3D('',#9362,#7524,#7525);
#6140=AXIS2_PLACEMENT_3D('',#9364,#7526,#7527);
#6141=AXIS2_PLACEMENT_3D('',#9366,#7528,#7529);
#6142=AXIS2_PLACEMENT_3D('',#9368,#7530,#7531);
#6143=AXIS2_PLACEMENT_3D('',#9370,#7532,#7533);
#6144=AXIS2_PLACEMENT_3D('',#9372,#7534,#7535);
#6145=AXIS2_PLACEMENT_3D('',#9374,#7536,#7537);
#6146=AXIS2_PLACEMENT_3D('',#9376,#7538,#7539);
#6147=AXIS2_PLACEMENT_3D('',#9378,#7540,#7541);
#6148=AXIS2_PLACEMENT_3D('',#9380,#7542,#7543);
#6149=AXIS2_PLACEMENT_3D('',#9382,#7544,#7545);
#6150=AXIS2_PLACEMENT_3D('',#9384,#7546,#7547);
#6151=AXIS2_PLACEMENT_3D('',#9386,#7548,#7549);
#6152=AXIS2_PLACEMENT_3D('',#9388,#7550,#7551);
#6153=AXIS2_PLACEMENT_3D('',#9390,#7552,#7553);
#6154=AXIS2_PLACEMENT_3D('',#9392,#7554,#7555);
#6155=AXIS2_PLACEMENT_3D('',#9394,#7556,#7557);
#6156=AXIS2_PLACEMENT_3D('',#9396,#7558,#7559);
#6157=AXIS2_PLACEMENT_3D('',#9398,#7560,#7561);
#6158=AXIS2_PLACEMENT_3D('',#9400,#7562,#7563);
#6159=AXIS2_PLACEMENT_3D('',#9402,#7564,#7565);
#6160=AXIS2_PLACEMENT_3D('',#9404,#7566,#7567);
#6161=AXIS2_PLACEMENT_3D('',#9406,#7568,#7569);
#6162=AXIS2_PLACEMENT_3D('',#9408,#7570,#7571);
#6163=AXIS2_PLACEMENT_3D('',#9410,#7572,#7573);
#6164=AXIS2_PLACEMENT_3D('',#9412,#7574,#7575);
#6165=AXIS2_PLACEMENT_3D('',#9414,#7576,#7577);
#6166=AXIS2_PLACEMENT_3D('',#9416,#7578,#7579);
#6167=AXIS2_PLACEMENT_3D('',#9418,#7580,#7581);
#6168=AXIS2_PLACEMENT_3D('',#9420,#7582,#7583);
#6169=AXIS2_PLACEMENT_3D('',#9421,#7584,#7585);
#6170=AXIS2_PLACEMENT_3D('',#9426,#7588,#7589);
#6171=AXIS2_PLACEMENT_3D('',#9427,#7590,#7591);
#6172=AXIS2_PLACEMENT_3D('',#9430,#7593,#7594);
#6173=AXIS2_PLACEMENT_3D('',#9433,#7596,#7597);
#6174=AXIS2_PLACEMENT_3D('',#9438,#7600,#7601);
#6175=AXIS2_PLACEMENT_3D('',#9439,#7602,#7603);
#6176=AXIS2_PLACEMENT_3D('',#9444,#7606,#7607);
#6177=AXIS2_PLACEMENT_3D('',#9445,#7608,#7609);
#6178=AXIS2_PLACEMENT_3D('',#9450,#7612,#7613);
#6179=AXIS2_PLACEMENT_3D('',#9451,#7614,#7615);
#6180=AXIS2_PLACEMENT_3D('',#9454,#7617,#7618);
#6181=AXIS2_PLACEMENT_3D('',#9457,#7620,#7621);
#6182=AXIS2_PLACEMENT_3D('',#9462,#7624,#7625);
#6183=AXIS2_PLACEMENT_3D('',#9463,#7626,#7627);
#6184=AXIS2_PLACEMENT_3D('',#9466,#7629,#7630);
#6185=AXIS2_PLACEMENT_3D('',#9469,#7632,#7633);
#6186=AXIS2_PLACEMENT_3D('',#9474,#7636,#7637);
#6187=AXIS2_PLACEMENT_3D('',#9475,#7638,#7639);
#6188=AXIS2_PLACEMENT_3D('',#9480,#7642,#7643);
#6189=AXIS2_PLACEMENT_3D('',#9481,#7644,#7645);
#6190=AXIS2_PLACEMENT_3D('',#9484,#7647,#7648);
#6191=AXIS2_PLACEMENT_3D('',#9487,#7650,#7651);
#6192=AXIS2_PLACEMENT_3D('',#9492,#7654,#7655);
#6193=AXIS2_PLACEMENT_3D('',#9493,#7656,#7657);
#6194=AXIS2_PLACEMENT_3D('',#9496,#7659,#7660);
#6195=AXIS2_PLACEMENT_3D('',#9499,#7662,#7663);
#6196=AXIS2_PLACEMENT_3D('',#9502,#7665,#7666);
#6197=AXIS2_PLACEMENT_3D('',#9505,#7668,#7669);
#6198=AXIS2_PLACEMENT_3D('',#9508,#7671,#7672);
#6199=AXIS2_PLACEMENT_3D('',#9511,#7674,#7675);
#6200=AXIS2_PLACEMENT_3D('',#9516,#7678,#7679);
#6201=AXIS2_PLACEMENT_3D('',#9517,#7680,#7681);
#6202=AXIS2_PLACEMENT_3D('',#9522,#7684,#7685);
#6203=AXIS2_PLACEMENT_3D('',#9523,#7686,#7687);
#6204=AXIS2_PLACEMENT_3D('',#9526,#7689,#7690);
#6205=AXIS2_PLACEMENT_3D('',#9529,#7692,#7693);
#6206=AXIS2_PLACEMENT_3D('',#9532,#7695,#7696);
#6207=AXIS2_PLACEMENT_3D('',#9535,#7698,#7699);
#6208=AXIS2_PLACEMENT_3D('',#9538,#7701,#7702);
#6209=AXIS2_PLACEMENT_3D('',#9541,#7704,#7705);
#6210=AXIS2_PLACEMENT_3D('',#9546,#7708,#7709);
#6211=AXIS2_PLACEMENT_3D('',#9547,#7710,#7711);
#6212=AXIS2_PLACEMENT_3D('',#9548,#7712,#7713);
#6213=AXIS2_PLACEMENT_3D('',#9550,#7714,#7715);
#6214=AXIS2_PLACEMENT_3D('',#9552,#7716,#7717);
#6215=AXIS2_PLACEMENT_3D('',#9554,#7718,#7719);
#6216=AXIS2_PLACEMENT_3D('',#9555,#7720,#7721);
#6217=AXIS2_PLACEMENT_3D('',#9557,#7722,#7723);
#6218=AXIS2_PLACEMENT_3D('',#9559,#7724,#7725);
#6219=AXIS2_PLACEMENT_3D('',#9560,#7726,#7727);
#6220=AXIS2_PLACEMENT_3D('',#9562,#7728,#7729);
#6221=AXIS2_PLACEMENT_3D('',#9564,#7730,#7731);
#6222=AXIS2_PLACEMENT_3D('',#9565,#7732,#7733);
#6223=AXIS2_PLACEMENT_3D('',#9567,#7734,#7735);
#6224=AXIS2_PLACEMENT_3D('',#9569,#7736,#7737);
#6225=AXIS2_PLACEMENT_3D('',#9570,#7738,#7739);
#6226=AXIS2_PLACEMENT_3D('',#9572,#7740,#7741);
#6227=AXIS2_PLACEMENT_3D('',#9574,#7742,#7743);
#6228=AXIS2_PLACEMENT_3D('',#9576,#7744,#7745);
#6229=AXIS2_PLACEMENT_3D('',#9578,#7746,#7747);
#6230=AXIS2_PLACEMENT_3D('',#9580,#7748,#7749);
#6231=AXIS2_PLACEMENT_3D('',#9582,#7750,#7751);
#6232=AXIS2_PLACEMENT_3D('',#9583,#7752,#7753);
#6233=AXIS2_PLACEMENT_3D('',#9585,#7754,#7755);
#6234=AXIS2_PLACEMENT_3D('',#9587,#7756,#7757);
#6235=AXIS2_PLACEMENT_3D('',#9588,#7758,#7759);
#6236=AXIS2_PLACEMENT_3D('',#9590,#7760,#7761);
#6237=AXIS2_PLACEMENT_3D('',#9592,#7762,#7763);
#6238=AXIS2_PLACEMENT_3D('',#9593,#7764,#7765);
#6239=AXIS2_PLACEMENT_3D('',#9595,#7766,#7767);
#6240=AXIS2_PLACEMENT_3D('',#9597,#7768,#7769);
#6241=AXIS2_PLACEMENT_3D('',#9598,#7770,#7771);
#6242=AXIS2_PLACEMENT_3D('',#9600,#7772,#7773);
#6243=AXIS2_PLACEMENT_3D('',#9602,#7774,#7775);
#6244=AXIS2_PLACEMENT_3D('',#9603,#7776,#7777);
#6245=AXIS2_PLACEMENT_3D('',#9605,#7778,#7779);
#6246=AXIS2_PLACEMENT_3D('',#9607,#7780,#7781);
#6247=AXIS2_PLACEMENT_3D('',#9608,#7782,#7783);
#6248=AXIS2_PLACEMENT_3D('',#9610,#7784,#7785);
#6249=AXIS2_PLACEMENT_3D('',#9612,#7786,#7787);
#6250=AXIS2_PLACEMENT_3D('',#9613,#7788,#7789);
#6251=AXIS2_PLACEMENT_3D('',#9615,#7790,#7791);
#6252=AXIS2_PLACEMENT_3D('',#9617,#7792,#7793);
#6253=AXIS2_PLACEMENT_3D('',#9618,#7794,#7795);
#6254=AXIS2_PLACEMENT_3D('',#9620,#7796,#7797);
#6255=AXIS2_PLACEMENT_3D('',#9622,#7798,#7799);
#6256=AXIS2_PLACEMENT_3D('',#9623,#7800,#7801);
#6257=AXIS2_PLACEMENT_3D('',#9625,#7802,#7803);
#6258=AXIS2_PLACEMENT_3D('',#9627,#7804,#7805);
#6259=AXIS2_PLACEMENT_3D('',#9628,#7806,#7807);
#6260=AXIS2_PLACEMENT_3D('',#9630,#7808,#7809);
#6261=AXIS2_PLACEMENT_3D('',#9632,#7810,#7811);
#6262=AXIS2_PLACEMENT_3D('',#9633,#7812,#7813);
#6263=AXIS2_PLACEMENT_3D('',#9635,#7814,#7815);
#6264=AXIS2_PLACEMENT_3D('',#9637,#7816,#7817);
#6265=AXIS2_PLACEMENT_3D('',#9638,#7818,#7819);
#6266=AXIS2_PLACEMENT_3D('',#9640,#7820,#7821);
#6267=AXIS2_PLACEMENT_3D('',#9642,#7822,#7823);
#6268=AXIS2_PLACEMENT_3D('',#9643,#7824,#7825);
#6269=AXIS2_PLACEMENT_3D('',#9645,#7826,#7827);
#6270=AXIS2_PLACEMENT_3D('',#9647,#7828,#7829);
#6271=AXIS2_PLACEMENT_3D('',#9648,#7830,#7831);
#6272=AXIS2_PLACEMENT_3D('',#9650,#7832,#7833);
#6273=AXIS2_PLACEMENT_3D('',#9652,#7834,#7835);
#6274=AXIS2_PLACEMENT_3D('',#9653,#7836,#7837);
#6275=AXIS2_PLACEMENT_3D('',#9655,#7838,#7839);
#6276=AXIS2_PLACEMENT_3D('',#9657,#7840,#7841);
#6277=AXIS2_PLACEMENT_3D('',#9658,#7842,#7843);
#6278=AXIS2_PLACEMENT_3D('',#9660,#7844,#7845);
#6279=AXIS2_PLACEMENT_3D('',#9661,#7846,#7847);
#6280=AXIS2_PLACEMENT_3D('',#9664,#7850,#7851);
#6281=AXIS2_PLACEMENT_3D('',#9666,#7853,#7854);
#6282=AXIS2_PLACEMENT_3D('',#9668,#7856,#7857);
#6283=AXIS2_PLACEMENT_3D('',#9669,#7858,#7859);
#6284=AXIS2_PLACEMENT_3D('',#9671,#7861,#7862);
#6285=AXIS2_PLACEMENT_3D('',#9673,#7864,#7865);
#6286=AXIS2_PLACEMENT_3D('',#9674,#7866,#7867);
#6287=AXIS2_PLACEMENT_3D('',#9676,#7869,#7870);
#6288=AXIS2_PLACEMENT_3D('',#9678,#7872,#7873);
#6289=AXIS2_PLACEMENT_3D('',#9679,#7874,#7875);
#6290=AXIS2_PLACEMENT_3D('',#9681,#7877,#7878);
#6291=AXIS2_PLACEMENT_3D('',#9683,#7880,#7881);
#6292=AXIS2_PLACEMENT_3D('',#9684,#7882,#7883);
#6293=AXIS2_PLACEMENT_3D('',#9686,#7885,#7886);
#6294=AXIS2_PLACEMENT_3D('',#9688,#7888,#7889);
#6295=AXIS2_PLACEMENT_3D('',#9689,#7890,#7891);
#6296=AXIS2_PLACEMENT_3D('',#9691,#7893,#7894);
#6297=AXIS2_PLACEMENT_3D('',#9693,#7896,#7897);
#6298=AXIS2_PLACEMENT_3D('',#9694,#7898,#7899);
#6299=AXIS2_PLACEMENT_3D('',#9696,#7901,#7902);
#6300=AXIS2_PLACEMENT_3D('',#9698,#7904,#7905);
#6301=AXIS2_PLACEMENT_3D('',#9699,#7906,#7907);
#6302=AXIS2_PLACEMENT_3D('',#9701,#7909,#7910);
#6303=AXIS2_PLACEMENT_3D('',#9703,#7912,#7913);
#6304=AXIS2_PLACEMENT_3D('',#9704,#7914,#7915);
#6305=AXIS2_PLACEMENT_3D('',#9706,#7917,#7918);
#6306=AXIS2_PLACEMENT_3D('',#9708,#7920,#7921);
#6307=AXIS2_PLACEMENT_3D('',#9709,#7922,#7923);
#6308=AXIS2_PLACEMENT_3D('',#9711,#7925,#7926);
#6309=AXIS2_PLACEMENT_3D('',#9713,#7928,#7929);
#6310=AXIS2_PLACEMENT_3D('',#9714,#7930,#7931);
#6311=AXIS2_PLACEMENT_3D('',#9716,#7933,#7934);
#6312=AXIS2_PLACEMENT_3D('',#9718,#7936,#7937);
#6313=AXIS2_PLACEMENT_3D('',#9719,#7938,#7939);
#6314=AXIS2_PLACEMENT_3D('',#9721,#7941,#7942);
#6315=AXIS2_PLACEMENT_3D('',#9723,#7944,#7945);
#6316=AXIS2_PLACEMENT_3D('',#9724,#7946,#7947);
#6317=AXIS2_PLACEMENT_3D('',#9726,#7949,#7950);
#6318=AXIS2_PLACEMENT_3D('',#9728,#7952,#7953);
#6319=AXIS2_PLACEMENT_3D('',#9729,#7954,#7955);
#6320=AXIS2_PLACEMENT_3D('',#9731,#7957,#7958);
#6321=AXIS2_PLACEMENT_3D('',#9733,#7960,#7961);
#6322=AXIS2_PLACEMENT_3D('',#9734,#7962,#7963);
#6323=AXIS2_PLACEMENT_3D('',#9736,#7965,#7966);
#6324=AXIS2_PLACEMENT_3D('',#9738,#7968,#7969);
#6325=AXIS2_PLACEMENT_3D('',#9739,#7970,#7971);
#6326=AXIS2_PLACEMENT_3D('',#9741,#7973,#7974);
#6327=AXIS2_PLACEMENT_3D('',#9743,#7976,#7977);
#6328=AXIS2_PLACEMENT_3D('',#9744,#7978,#7979);
#6329=AXIS2_PLACEMENT_3D('',#9746,#7981,#7982);
#6330=AXIS2_PLACEMENT_3D('',#9748,#7984,#7985);
#6331=AXIS2_PLACEMENT_3D('',#9749,#7986,#7987);
#6332=AXIS2_PLACEMENT_3D('',#9751,#7989,#7990);
#6333=AXIS2_PLACEMENT_3D('',#9753,#7992,#7993);
#6334=AXIS2_PLACEMENT_3D('',#9754,#7994,#7995);
#6335=AXIS2_PLACEMENT_3D('',#9756,#7997,#7998);
#6336=AXIS2_PLACEMENT_3D('',#9758,#8000,#8001);
#6337=AXIS2_PLACEMENT_3D('',#9759,#8002,#8003);
#6338=AXIS2_PLACEMENT_3D('',#9761,#8005,#8006);
#6339=AXIS2_PLACEMENT_3D('',#9763,#8008,#8009);
#6340=AXIS2_PLACEMENT_3D('',#9764,#8010,#8011);
#6341=AXIS2_PLACEMENT_3D('',#9766,#8013,#8014);
#6342=AXIS2_PLACEMENT_3D('',#9768,#8016,#8017);
#6343=AXIS2_PLACEMENT_3D('',#9769,#8018,#8019);
#6344=AXIS2_PLACEMENT_3D('',#9771,#8021,#8022);
#6345=AXIS2_PLACEMENT_3D('',#9773,#8024,#8025);
#6346=AXIS2_PLACEMENT_3D('',#9774,#8026,#8027);
#6347=AXIS2_PLACEMENT_3D('',#9775,#8028,#8029);
#6348=AXIS2_PLACEMENT_3D('',#9777,#8030,#8031);
#6349=AXIS2_PLACEMENT_3D('',#9779,#8032,#8033);
#6350=AXIS2_PLACEMENT_3D('',#9780,#8034,#8035);
#6351=AXIS2_PLACEMENT_3D('',#9782,#8036,#8037);
#6352=AXIS2_PLACEMENT_3D('',#9783,#8038,#8039);
#6353=AXIS2_PLACEMENT_3D('',#9784,#8040,#8041);
#6354=AXIS2_PLACEMENT_3D('',#9785,#8042,#8043);
#6355=AXIS2_PLACEMENT_3D('',#9787,#8044,#8045);
#6356=AXIS2_PLACEMENT_3D('',#9789,#8046,#8047);
#6357=AXIS2_PLACEMENT_3D('',#9790,#8048,#8049);
#6358=AXIS2_PLACEMENT_3D('',#9792,#8050,#8051);
#6359=AXIS2_PLACEMENT_3D('',#9793,#8052,#8053);
#6360=AXIS2_PLACEMENT_3D('',#9794,#8054,#8055);
#6361=AXIS2_PLACEMENT_3D('',#9795,#8056,#8057);
#6362=AXIS2_PLACEMENT_3D('',#9796,#8058,#8059);
#6363=AXIS2_PLACEMENT_3D('',#9801,#8061,#8062);
#6364=AXIS2_PLACEMENT_3D('',#9804,#8064,#8065);
#6365=AXIS2_PLACEMENT_3D('',#9805,#8066,#8067);
#6366=AXIS2_PLACEMENT_3D('',#9809,#8069,#8070);
#6367=AXIS2_PLACEMENT_3D('',#9810,#8071,#8072);
#6368=AXIS2_PLACEMENT_3D('',#9811,#8073,#8074);
#6369=AXIS2_PLACEMENT_3D('',#9815,#8076,#8077);
#6370=AXIS2_PLACEMENT_3D('',#9816,#8078,#8079);
#6371=AXIS2_PLACEMENT_3D('',#9819,#8082,#8083);
#6372=AXIS2_PLACEMENT_3D('',#9820,#8084,#8085);
#6373=AXIS2_PLACEMENT_3D('',#9822,#8086,#8087);
#6374=AXIS2_PLACEMENT_3D('',#9823,#8088,#8089);
#6375=AXIS2_PLACEMENT_3D('',#9825,#8090,#8091);
#6376=AXIS2_PLACEMENT_3D('',#9826,#8092,#8093);
#6377=AXIS2_PLACEMENT_3D('',#9827,#8094,#8095);
#6378=AXIS2_PLACEMENT_3D('',#9828,#8096,#8097);
#6379=AXIS2_PLACEMENT_3D('',#9831,#8098,#8099);
#6380=AXIS2_PLACEMENT_3D('',#9841,#8100,#8101);
#6381=AXIS2_PLACEMENT_3D('',#9842,#8102,#8103);
#6382=AXIS2_PLACEMENT_3D('',#9845,#8105,#8106);
#6383=AXIS2_PLACEMENT_3D('',#9848,#8108,#8109);
#6384=AXIS2_PLACEMENT_3D('',#9849,#8110,#8111);
#6385=AXIS2_PLACEMENT_3D('',#9851,#8112,#8113);
#6386=AXIS2_PLACEMENT_3D('',#9860,#8114,#8115);
#6387=AXIS2_PLACEMENT_3D('',#9863,#8118,#8119);
#6388=AXIS2_PLACEMENT_3D('',#9884,#8122,#8123);
#6389=AXIS2_PLACEMENT_3D('',#9885,#8124,#8125);
#6390=AXIS2_PLACEMENT_3D('',#9890,#8127,#8128);
#6391=AXIS2_PLACEMENT_3D('',#9893,#8130,#8131);
#6392=AXIS2_PLACEMENT_3D('',#9894,#8132,#8133);
#6393=AXIS2_PLACEMENT_3D('',#9895,#8134,#8135);
#6394=AXIS2_PLACEMENT_3D('',#9896,#8136,#8137);
#6395=AXIS2_PLACEMENT_3D('',#9897,#8138,#8139);
#6396=AXIS2_PLACEMENT_3D('',#9898,#8140,#8141);
#6397=AXIS2_PLACEMENT_3D('',#9899,#8142,#8143);
#6398=AXIS2_PLACEMENT_3D('',#9900,#8144,#8145);
#6399=AXIS2_PLACEMENT_3D('',#9901,#8146,#8147);
#6400=AXIS2_PLACEMENT_3D('',#9902,#8148,#8149);
#6401=AXIS2_PLACEMENT_3D('',#9903,#8150,#8151);
#6402=AXIS2_PLACEMENT_3D('',#9904,#8152,#8153);
#6403=AXIS2_PLACEMENT_3D('',#9906,#8154,#8155);
#6404=AXIS2_PLACEMENT_3D('',#9911,#8157,#8158);
#6405=AXIS2_PLACEMENT_3D('',#9914,#8160,#8161);
#6406=AXIS2_PLACEMENT_3D('',#9916,#8162,#8163);
#6407=AXIS2_PLACEMENT_3D('',#9917,#8164,#8165);
#6408=AXIS2_PLACEMENT_3D('',#9922,#8167,#8168);
#6409=AXIS2_PLACEMENT_3D('',#9925,#8170,#8171);
#6410=AXIS2_PLACEMENT_3D('',#9927,#8172,#8173);
#6411=AXIS2_PLACEMENT_3D('',#9929,#8174,#8175);
#6412=AXIS2_PLACEMENT_3D('',#9932,#8178,#8179);
#6413=AXIS2_PLACEMENT_3D('',#9934,#8181,#8182);
#6414=AXIS2_PLACEMENT_3D('',#9936,#8184,#8185);
#6415=AXIS2_PLACEMENT_3D('',#9937,#8186,#8187);
#6416=AXIS2_PLACEMENT_3D('',#9938,#8188,#8189);
#6417=AXIS2_PLACEMENT_3D('',#9939,#8190,#8191);
#6418=AXIS2_PLACEMENT_3D('',#9940,#8192,#8193);
#6419=AXIS2_PLACEMENT_3D('',#9941,#8194,#8195);
#6420=AXIS2_PLACEMENT_3D('',#9943,#8196,#8197);
#6421=AXIS2_PLACEMENT_3D('',#9945,#8198,#8199);
#6422=AXIS2_PLACEMENT_3D('',#9946,#8200,#8201);
#6423=AXIS2_PLACEMENT_3D('',#9948,#8202,#8203);
#6424=AXIS2_PLACEMENT_3D('',#9949,#8204,#8205);
#6425=AXIS2_PLACEMENT_3D('',#9951,#8206,#8207);
#6426=AXIS2_PLACEMENT_3D('',#9952,#8208,#8209);
#6427=AXIS2_PLACEMENT_3D('',#9954,#8210,#8211);
#6428=AXIS2_PLACEMENT_3D('',#9955,#8212,#8213);
#6429=AXIS2_PLACEMENT_3D('',#9957,#8214,#8215);
#6430=AXIS2_PLACEMENT_3D('',#9958,#8216,#8217);
#6431=AXIS2_PLACEMENT_3D('',#9960,#8218,#8219);
#6432=AXIS2_PLACEMENT_3D('',#9962,#8220,#8221);
#6433=AXIS2_PLACEMENT_3D('',#9963,#8222,#8223);
#6434=AXIS2_PLACEMENT_3D('',#9965,#8224,#8225);
#6435=AXIS2_PLACEMENT_3D('',#9967,#8226,#8227);
#6436=AXIS2_PLACEMENT_3D('',#9968,#8228,#8229);
#6437=AXIS2_PLACEMENT_3D('',#9970,#8230,#8231);
#6438=AXIS2_PLACEMENT_3D('',#9972,#8232,#8233);
#6439=AXIS2_PLACEMENT_3D('',#9973,#8234,#8235);
#6440=AXIS2_PLACEMENT_3D('',#9974,#8236,#8237);
#6441=AXIS2_PLACEMENT_3D('',#9976,#8238,#8239);
#6442=AXIS2_PLACEMENT_3D('',#9977,#8240,#8241);
#6443=AXIS2_PLACEMENT_3D('',#9978,#8242,#8243);
#6444=AXIS2_PLACEMENT_3D('',#9980,#8244,#8245);
#6445=AXIS2_PLACEMENT_3D('',#9981,#8246,#8247);
#6446=AXIS2_PLACEMENT_3D('',#9983,#8248,#8249);
#6447=AXIS2_PLACEMENT_3D('',#9984,#8250,#8251);
#6448=AXIS2_PLACEMENT_3D('',#9986,#8252,#8253);
#6449=AXIS2_PLACEMENT_3D('',#9987,#8254,#8255);
#6450=AXIS2_PLACEMENT_3D('',#9988,#8256,#8257);
#6451=AXIS2_PLACEMENT_3D('',#9989,#8258,#8259);
#6452=AXIS2_PLACEMENT_3D('',#9990,#8260,#8261);
#6453=AXIS2_PLACEMENT_3D('',#9993,#8262,#8263);
#6454=AXIS2_PLACEMENT_3D('',#9997,#8265,#8266);
#6455=AXIS2_PLACEMENT_3D('',#10003,#8269,#8270);
#6456=AXIS2_PLACEMENT_3D('',#10007,#8272,#8273);
#6457=AXIS2_PLACEMENT_3D('',#10009,#8274,#8275);
#6458=AXIS2_PLACEMENT_3D('',#10012,#8277,#8278);
#6459=AXIS2_PLACEMENT_3D('',#10014,#8279,#8280);
#6460=AXIS2_PLACEMENT_3D('',#10015,#8281,#8282);
#6461=AXIS2_PLACEMENT_3D('',#10020,#8284,#8285);
#6462=AXIS2_PLACEMENT_3D('',#10022,#8286,#8287);
#6463=AXIS2_PLACEMENT_3D('',#10026,#8289,#8290);
#6464=AXIS2_PLACEMENT_3D('',#10032,#8293,#8294);
#6465=AXIS2_PLACEMENT_3D('',#10036,#8296,#8297);
#6466=AXIS2_PLACEMENT_3D('',#10037,#8298,#8299);
#6467=AXIS2_PLACEMENT_3D('',#10039,#8300,#8301);
#6468=AXIS2_PLACEMENT_3D('',#10042,#8304,#8305);
#6469=AXIS2_PLACEMENT_3D('',#10044,#8307,#8308);
#6470=AXIS2_PLACEMENT_3D('',#10046,#8310,#8311);
#6471=AXIS2_PLACEMENT_3D('',#10048,#8313,#8314);
#6472=AXIS2_PLACEMENT_3D('',#10050,#8316,#8317);
#6473=AXIS2_PLACEMENT_3D('',#10052,#8319,#8320);
#6474=AXIS2_PLACEMENT_3D('',#10054,#8322,#8323);
#6475=AXIS2_PLACEMENT_3D('',#10056,#8325,#8326);
#6476=AXIS2_PLACEMENT_3D('',#10058,#8328,#8329);
#6477=AXIS2_PLACEMENT_3D('',#10060,#8331,#8332);
#6478=AXIS2_PLACEMENT_3D('',#10061,#8333,#8334);
#6479=AXIS2_PLACEMENT_3D('',#10062,#8335,#8336);
#6480=AXIS2_PLACEMENT_3D('',#10063,#8337,#8338);
#6481=AXIS2_PLACEMENT_3D('',#10067,#8340,#8341);
#6482=AXIS2_PLACEMENT_3D('',#10068,#8342,#8343);
#6483=AXIS2_PLACEMENT_3D('',#10069,#8344,#8345);
#6484=AXIS2_PLACEMENT_3D('',#10077,#8346,#8347);
#6485=AXIS2_PLACEMENT_3D('',#10083,#8348,#8349);
#6486=AXIS2_PLACEMENT_3D('',#10084,#8350,#8351);
#6487=AXIS2_PLACEMENT_3D('',#10086,#8352,#8353);
#6488=AXIS2_PLACEMENT_3D('',#10088,#8354,#8355);
#6489=AXIS2_PLACEMENT_3D('',#10089,#8356,#8357);
#6490=AXIS2_PLACEMENT_3D('',#10091,#8358,#8359);
#6491=AXIS2_PLACEMENT_3D('',#10093,#8361,#8362);
#6492=AXIS2_PLACEMENT_3D('',#10094,#8363,#8364);
#6493=AXIS2_PLACEMENT_3D('',#10102,#8365,#8366);
#6494=AXIS2_PLACEMENT_3D('',#10113,#8367,#8368);
#6495=AXIS2_PLACEMENT_3D('',#10119,#8369,#8370);
#6496=AXIS2_PLACEMENT_3D('',#10121,#8371,#8372);
#6497=AXIS2_PLACEMENT_3D('',#10122,#8373,#8374);
#6498=AXIS2_PLACEMENT_3D('',#10124,#8375,#8376);
#6499=AXIS2_PLACEMENT_3D('',#10125,#8377,#8378);
#6500=AXIS2_PLACEMENT_3D('',#10134,#8379,#8380);
#6501=AXIS2_PLACEMENT_3D('',#10137,#8383,#8384);
#6502=AXIS2_PLACEMENT_3D('',#10138,#8385,#8386);
#6503=AXIS2_PLACEMENT_3D('',#10139,#8387,#8388);
#6504=AXIS2_PLACEMENT_3D('',#10140,#8389,#8390);
#6505=DIRECTION('',(0.,0.,1.));
#6506=DIRECTION('',(1.,0.,0.));
#6507=DIRECTION('',(0.,-1.,0.));
#6508=DIRECTION('',(0.,0.,-1.));
#6509=DIRECTION('',(0.,-1.,0.));
#6510=DIRECTION('',(0.,0.,-1.));
#6511=DIRECTION('',(0.,1.,0.));
#6512=DIRECTION('',(0.,0.,1.));
#6513=DIRECTION('',(0.,-1.,0.));
#6514=DIRECTION('',(0.,0.,-1.));
#6515=DIRECTION('',(0.,1.,0.));
#6516=DIRECTION('',(1.,0.,0.));
#6517=DIRECTION('',(0.,1.,0.));
#6518=DIRECTION('',(0.,0.,1.));
#6519=DIRECTION('',(0.,1.,0.));
#6520=DIRECTION('',(0.,0.,1.));
#6521=DIRECTION('',(0.,1.,0.));
#6522=DIRECTION('',(0.,0.,1.));
#6523=DIRECTION('',(0.,1.,0.));
#6524=DIRECTION('',(0.,0.,1.));
#6525=DIRECTION('',(0.,1.,0.));
#6526=DIRECTION('',(0.,0.,1.));
#6527=DIRECTION('',(0.,1.,0.));
#6528=DIRECTION('',(0.,0.,1.));
#6529=DIRECTION('',(0.,1.,0.));
#6530=DIRECTION('',(0.,0.,1.));
#6531=DIRECTION('',(0.,1.,0.));
#6532=DIRECTION('',(0.,0.,1.));
#6533=DIRECTION('',(0.,1.,0.));
#6534=DIRECTION('',(0.,0.,1.));
#6535=DIRECTION('',(0.,1.,0.));
#6536=DIRECTION('',(0.,0.,1.));
#6537=DIRECTION('',(0.,1.,0.));
#6538=DIRECTION('',(0.,0.,1.));
#6539=DIRECTION('',(0.,-1.,0.));
#6540=DIRECTION('',(0.,0.,-1.));
#6541=DIRECTION('',(0.,-1.,0.));
#6542=DIRECTION('',(0.,0.,-1.));
#6543=DIRECTION('',(0.,-1.,0.));
#6544=DIRECTION('',(0.,0.,-1.));
#6545=DIRECTION('',(0.,-1.,0.));
#6546=DIRECTION('',(0.,0.,-1.));
#6547=DIRECTION('',(0.,-1.,0.));
#6548=DIRECTION('',(0.,0.,-1.));
#6549=DIRECTION('',(0.,0.,-1.));
#6550=DIRECTION('',(-1.,0.,0.));
#6551=DIRECTION('',(0.,1.,0.));
#6552=DIRECTION('',(0.,0.,1.));
#6553=DIRECTION('',(0.,1.,0.));
#6554=DIRECTION('',(0.,0.,1.));
#6555=DIRECTION('',(0.,1.,0.));
#6556=DIRECTION('',(0.,0.,1.));
#6557=DIRECTION('',(0.,1.,0.));
#6558=DIRECTION('',(0.,0.,1.));
#6559=DIRECTION('',(0.195284380651566,-0.980746659781992,-7.20111324682445E-17));
#6560=DIRECTION('',(0.980746659781992,0.195284380651566,-4.8095693299403E-17));
#6561=DIRECTION('',(0.,0.,-1.));
#6562=DIRECTION('',(-1.,0.,0.));
#6563=DIRECTION('',(1.,0.,0.));
#6564=DIRECTION('',(0.,0.,-1.));
#6565=DIRECTION('',(-1.,0.,0.));
#6566=DIRECTION('',(0.,0.,-1.));
#6567=DIRECTION('',(-1.,0.,0.));
#6568=DIRECTION('',(0.,0.,1.));
#6569=DIRECTION('',(1.,0.,0.));
#6570=DIRECTION('',(0.,0.,-1.));
#6571=DIRECTION('',(-1.,0.,0.));
#6572=DIRECTION('',(0.,0.,-1.));
#6573=DIRECTION('',(-1.,0.,0.));
#6574=DIRECTION('',(0.,0.,1.));
#6575=DIRECTION('',(1.,0.,0.));
#6576=DIRECTION('',(0.,0.,-1.));
#6577=DIRECTION('',(-1.,0.,0.));
#6578=DIRECTION('',(0.,0.,1.));
#6579=DIRECTION('',(1.,0.,0.));
#6580=DIRECTION('',(0.,0.,1.));
#6581=DIRECTION('',(1.,0.,0.));
#6582=DIRECTION('',(0.,0.,-1.));
#6583=DIRECTION('',(-1.,0.,0.));
#6584=DIRECTION('',(1.,0.,0.));
#6585=DIRECTION('',(0.,0.,-1.));
#6586=DIRECTION('',(-1.,0.,0.));
#6587=DIRECTION('',(0.,0.,1.));
#6588=DIRECTION('',(1.,0.,0.));
#6589=DIRECTION('',(0.,0.,1.));
#6590=DIRECTION('',(1.,0.,0.));
#6591=DIRECTION('',(0.,0.,1.));
#6592=DIRECTION('',(1.,0.,0.));
#6593=DIRECTION('',(0.,0.,-1.));
#6594=DIRECTION('',(-1.,0.,0.));
#6595=DIRECTION('',(0.,0.,1.));
#6596=DIRECTION('',(1.,0.,0.));
#6597=DIRECTION('',(0.,0.,-1.));
#6598=DIRECTION('',(-1.,0.,0.));
#6599=DIRECTION('',(0.,0.,-1.));
#6600=DIRECTION('',(-1.,0.,0.));
#6601=DIRECTION('',(0.,0.,-1.));
#6602=DIRECTION('',(-1.,0.,0.));
#6603=DIRECTION('',(0.,0.,1.));
#6604=DIRECTION('',(1.,0.,0.));
#6605=DIRECTION('',(1.,0.,0.));
#6606=DIRECTION('',(1.,0.,0.));
#6607=DIRECTION('',(0.,-1.,0.));
#6608=DIRECTION('',(0.,0.,-1.));
#6609=DIRECTION('',(0.,-1.,0.));
#6610=DIRECTION('',(0.,0.,-1.));
#6611=DIRECTION('',(0.,0.,1.));
#6612=DIRECTION('',(1.,0.,0.));
#6613=DIRECTION('',(-4.38440469925874E-17,-3.37314196379993E-16,1.));
#6614=DIRECTION('',(0.156844626527355,-0.987623290090657,-3.26262653247095E-16));
#6615=DIRECTION('',(4.20741553168916E-17,-1.96805055665783E-16,1.));
#6616=DIRECTION('',(0.992251237473569,-0.124247662884138,-6.62007008890971E-17));
#6617=DIRECTION('',(0.,-1.,0.));
#6618=DIRECTION('',(0.,0.,-1.));
#6619=DIRECTION('',(0.,1.,0.));
#6620=DIRECTION('',(0.,0.,1.));
#6621=DIRECTION('',(-1.21904419394898E-29,-1.,3.49148133884314E-15));
#6622=DIRECTION('',(0.,1.,0.));
#6623=DIRECTION('',(0.,0.,1.));
#6624=DIRECTION('',(0.,-1.,0.));
#6625=DIRECTION('',(0.,-1.,0.));
#6626=DIRECTION('',(0.,0.,-1.));
#6627=DIRECTION('',(0.,1.,0.));
#6628=DIRECTION('',(0.,0.,1.));
#6629=DIRECTION('',(-1.21904419394898E-29,-1.,3.49148133884314E-15));
#6630=DIRECTION('',(0.,1.,0.));
#6631=DIRECTION('',(0.,0.,1.));
#6632=DIRECTION('',(0.,-1.,0.));
#6633=DIRECTION('',(0.,-1.,0.));
#6634=DIRECTION('',(0.,0.,-1.));
#6635=DIRECTION('',(0.,1.,0.));
#6636=DIRECTION('',(0.,0.,1.));
#6637=DIRECTION('',(0.,1.,0.));
#6638=DIRECTION('',(0.,0.,1.));
#6639=DIRECTION('',(0.,1.,0.));
#6640=DIRECTION('',(0.,0.,1.));
#6641=DIRECTION('',(1.,0.,0.));
#6642=DIRECTION('',(0.,1.,0.));
#6643=DIRECTION('',(0.,0.,1.));
#6644=DIRECTION('',(-1.,0.,0.));
#6645=DIRECTION('',(0.,1.,0.));
#6646=DIRECTION('',(0.,0.,1.));
#6647=DIRECTION('',(-1.21904419394898E-29,-1.,3.49148133884314E-15));
#6648=DIRECTION('',(0.991444861373811,-4.55729764366563E-16,-0.130526192220048));
#6649=DIRECTION('',(-1.21904419394898E-29,-1.,3.49148133884314E-15));
#6650=DIRECTION('',(0.991444861373811,-4.55729764366563E-16,-0.130526192220048));
#6651=DIRECTION('',(-1.21904419394898E-29,-1.,3.49148133884314E-15));
#6652=DIRECTION('',(0.991444861373811,-4.55729764366563E-16,-0.130526192220048));
#6653=DIRECTION('',(0.,1.,0.));
#6654=DIRECTION('',(0.,0.,1.));
#6655=DIRECTION('',(-1.21904419394898E-29,-1.,3.49148133884314E-15));
#6656=DIRECTION('',(0.965925826289069,-9.03661866112653E-16,-0.258819045102518));
#6657=DIRECTION('',(-1.21904419394898E-29,-1.,3.49148133884314E-15));
#6658=DIRECTION('',(0.965925826289069,-9.03661866112653E-16,-0.258819045102518));
#6659=DIRECTION('',(-1.21904419394898E-29,-1.,3.49148133884314E-15));
#6660=DIRECTION('',(0.965925826289069,-9.03661866112653E-16,-0.258819045102518));
#6661=DIRECTION('',(0.,1.,0.));
#6662=DIRECTION('',(0.,0.,1.));
#6663=DIRECTION('',(-1.21904419394898E-29,-1.,3.49148133884314E-15));
#6664=DIRECTION('',(0.923879532511288,-1.33613206278715E-15,-0.382683432365088));
#6665=DIRECTION('',(-1.21904419394898E-29,-1.,3.49148133884314E-15));
#6666=DIRECTION('',(0.923879532511288,-1.33613206278715E-15,-0.382683432365088));
#6667=DIRECTION('',(-1.21904419394898E-29,-1.,3.49148133884314E-15));
#6668=DIRECTION('',(0.923879532511288,-1.33613206278715E-15,-0.382683432365088));
#6669=DIRECTION('',(0.,1.,0.));
#6670=DIRECTION('',(0.,0.,1.));
#6671=DIRECTION('',(-1.21904419394898E-29,-1.,3.49148133884314E-15));
#6672=DIRECTION('',(0.86602540378444,-1.74574066942157E-15,-0.5));
#6673=DIRECTION('',(-1.21904419394898E-29,-1.,3.49148133884314E-15));
#6674=DIRECTION('',(0.86602540378444,-1.74574066942157E-15,-0.5));
#6675=DIRECTION('',(-1.21904419394898E-29,-1.,3.49148133884314E-15));
#6676=DIRECTION('',(0.86602540378444,-1.74574066942157E-15,-0.5));
#6677=DIRECTION('',(0.,1.,0.));
#6678=DIRECTION('',(0.,0.,1.));
#6679=DIRECTION('',(-1.21904419394898E-29,-1.,3.49148133884314E-15));
#6680=DIRECTION('',(0.793353340291236,-2.12547916919143E-15,-0.608761429008719));
#6681=DIRECTION('',(-1.21904419394898E-29,-1.,3.49148133884314E-15));
#6682=DIRECTION('',(0.793353340291236,-2.12547916919143E-15,-0.608761429008719));
#6683=DIRECTION('',(-1.21904419394898E-29,-1.,3.49148133884314E-15));
#6684=DIRECTION('',(0.793353340291236,-2.12547916919143E-15,-0.608761429008719));
#6685=DIRECTION('',(0.,1.,0.));
#6686=DIRECTION('',(0.,0.,1.));
#6687=DIRECTION('',(-1.21904419394898E-29,-1.,3.49148133884314E-15));
#6688=DIRECTION('',(0.707106781186549,-2.46885013108227E-15,-0.707106781186547));
#6689=DIRECTION('',(-1.21904419394898E-29,-1.,3.49148133884314E-15));
#6690=DIRECTION('',(0.707106781186549,-2.46885013108227E-15,-0.707106781186547));
#6691=DIRECTION('',(-1.21904419394898E-29,-1.,3.49148133884314E-15));
#6692=DIRECTION('',(0.707106781186549,-2.46885013108227E-15,-0.707106781186547));
#6693=DIRECTION('',(0.,1.,0.));
#6694=DIRECTION('',(0.,0.,1.));
#6695=DIRECTION('',(-1.21904419394898E-29,-1.,3.49148133884314E-15));
#6696=DIRECTION('',(0.608761429008722,-2.76997838273572E-15,-0.793353340291234));
#6697=DIRECTION('',(-1.21904419394898E-29,-1.,3.49148133884314E-15));
#6698=DIRECTION('',(0.608761429008722,-2.76997838273572E-15,-0.793353340291234));
#6699=DIRECTION('',(-1.21904419394898E-29,-1.,3.49148133884314E-15));
#6700=DIRECTION('',(0.608761429008722,-2.76997838273572E-15,-0.793353340291234));
#6701=DIRECTION('',(0.,1.,0.));
#6702=DIRECTION('',(0.,0.,1.));
#6703=DIRECTION('',(-1.21904419394898E-29,-1.,3.49148133884314E-15));
#6704=DIRECTION('',(0.5,-3.02371153627746E-15,-0.866025403784438));
#6705=DIRECTION('',(-1.21904419394898E-29,-1.,3.49148133884314E-15));
#6706=DIRECTION('',(0.5,-3.02371153627746E-15,-0.866025403784438));
#6707=DIRECTION('',(-1.21904419394898E-29,-1.,3.49148133884314E-15));
#6708=DIRECTION('',(0.5,-3.02371153627746E-15,-0.866025403784438));
#6709=DIRECTION('',(0.,1.,0.));
#6710=DIRECTION('',(0.,0.,1.));
#6711=DIRECTION('',(-1.21904419394898E-29,-1.,3.49148133884314E-15));
#6712=DIRECTION('',(0.382683432365091,-3.22570814710228E-15,-0.923879532511286));
#6713=DIRECTION('',(-1.21904419394898E-29,-1.,3.49148133884314E-15));
#6714=DIRECTION('',(0.382683432365091,-3.22570814710228E-15,-0.923879532511286));
#6715=DIRECTION('',(-1.21904419394898E-29,-1.,3.49148133884314E-15));
#6716=DIRECTION('',(0.382683432365091,-3.22570814710228E-15,-0.923879532511286));
#6717=DIRECTION('',(0.,1.,0.));
#6718=DIRECTION('',(0.,0.,1.));
#6719=DIRECTION('',(-1.21904419394898E-29,-1.,3.49148133884314E-15));
#6720=DIRECTION('',(0.258819045102522,-3.37251199719492E-15,-0.965925826289068));
#6721=DIRECTION('',(-1.21904419394898E-29,-1.,3.49148133884314E-15));
#6722=DIRECTION('',(0.258819045102522,-3.37251199719492E-15,-0.965925826289068));
#6723=DIRECTION('',(-1.21904419394898E-29,-1.,3.49148133884314E-15));
#6724=DIRECTION('',(0.258819045102522,-3.37251199719492E-15,-0.965925826289068));
#6725=DIRECTION('',(0.,1.,0.));
#6726=DIRECTION('',(0.,0.,1.));
#6727=DIRECTION('',(-1.21904419394898E-29,-1.,3.49148133884314E-15));
#6728=DIRECTION('',(0.130526192220052,-3.46161123197858E-15,-0.99144486137381));
#6729=DIRECTION('',(-1.21904419394898E-29,-1.,3.49148133884314E-15));
#6730=DIRECTION('',(0.130526192220052,-3.46161123197858E-15,-0.99144486137381));
#6731=DIRECTION('',(-1.21904419394898E-29,-1.,3.49148133884314E-15));
#6732=DIRECTION('',(0.130526192220052,-3.46161123197858E-15,-0.99144486137381));
#6733=DIRECTION('',(0.866025403784439,0.,0.5));
#6734=DIRECTION('',(0.,1.,0.));
#6735=DIRECTION('',(0.,0.,1.));
#6736=DIRECTION('',(1.,0.,-1.91967175081904E-16));
#6737=DIRECTION('',(0.,1.,0.));
#6738=DIRECTION('',(0.,0.,1.));
#6739=DIRECTION('',(-1.,0.,0.));
#6740=DIRECTION('',(0.,-1.,0.));
#6741=DIRECTION('',(0.,0.,1.));
#6742=DIRECTION('',(0.,-1.,0.));
#6743=DIRECTION('',(0.,0.,1.));
#6744=DIRECTION('',(0.,1.,0.));
#6745=DIRECTION('',(0.,0.,1.));
#6746=DIRECTION('',(0.,1.,0.));
#6747=DIRECTION('',(0.,0.,1.));
#6748=DIRECTION('',(0.,-1.,0.));
#6749=DIRECTION('',(0.,0.,1.));
#6750=DIRECTION('',(0.,-1.,0.));
#6751=DIRECTION('',(0.,0.,1.));
#6752=DIRECTION('',(-1.,0.,0.));
#6753=DIRECTION('',(0.,1.,0.));
#6754=DIRECTION('',(0.,0.,1.));
#6755=DIRECTION('',(1.,0.,-1.91967175081904E-16));
#6756=DIRECTION('',(0.,1.,0.));
#6757=DIRECTION('',(0.,0.,1.));
#6758=DIRECTION('',(0.866025403784439,0.,0.5));
#6759=DIRECTION('',(0.,1.,0.));
#6760=DIRECTION('',(0.,0.,1.));
#6761=DIRECTION('',(0.,1.,0.));
#6762=DIRECTION('',(0.,0.,1.));
#6763=DIRECTION('',(0.,1.,0.));
#6764=DIRECTION('',(0.,0.,1.));
#6765=DIRECTION('',(0.,1.,0.));
#6766=DIRECTION('',(0.,0.,1.));
#6767=DIRECTION('',(0.,1.,0.));
#6768=DIRECTION('',(0.,0.,1.));
#6769=DIRECTION('',(0.,1.,0.));
#6770=DIRECTION('',(0.,0.,1.));
#6771=DIRECTION('',(0.,1.,0.));
#6772=DIRECTION('',(0.,0.,1.));
#6773=DIRECTION('',(0.,1.,0.));
#6774=DIRECTION('',(0.,0.,1.));
#6775=DIRECTION('',(0.,1.,0.));
#6776=DIRECTION('',(0.,0.,1.));
#6777=DIRECTION('',(0.,1.,0.));
#6778=DIRECTION('',(0.,0.,1.));
#6779=DIRECTION('',(0.,1.,0.));
#6780=DIRECTION('',(0.,0.,1.));
#6781=DIRECTION('',(0.,1.,0.));
#6782=DIRECTION('',(0.,0.,1.));
#6783=DIRECTION('',(0.,1.,0.));
#6784=DIRECTION('',(0.,0.,1.));
#6785=DIRECTION('',(0.,1.,0.));
#6786=DIRECTION('',(0.,0.,1.));
#6787=DIRECTION('',(0.,1.,0.));
#6788=DIRECTION('',(0.,0.,1.));
#6789=DIRECTION('',(0.,1.,0.));
#6790=DIRECTION('',(0.,0.,1.));
#6791=DIRECTION('',(0.,1.,0.));
#6792=DIRECTION('',(0.,0.,1.));
#6793=DIRECTION('',(0.,1.,0.));
#6794=DIRECTION('',(0.,0.,1.));
#6795=DIRECTION('',(0.,1.,0.));
#6796=DIRECTION('',(0.,0.,1.));
#6797=DIRECTION('',(0.,1.,0.));
#6798=DIRECTION('',(0.,0.,1.));
#6799=DIRECTION('',(0.,1.,0.));
#6800=DIRECTION('',(0.,0.,1.));
#6801=DIRECTION('',(0.,1.,0.));
#6802=DIRECTION('',(0.,0.,1.));
#6803=DIRECTION('',(0.,1.,0.));
#6804=DIRECTION('',(0.,0.,1.));
#6805=DIRECTION('',(0.,1.,0.));
#6806=DIRECTION('',(0.,0.,1.));
#6807=DIRECTION('',(0.,1.,0.));
#6808=DIRECTION('',(0.,0.,1.));
#6809=DIRECTION('',(0.,1.,0.));
#6810=DIRECTION('',(0.,0.,1.));
#6811=DIRECTION('',(0.,1.,0.));
#6812=DIRECTION('',(0.,0.,1.));
#6813=DIRECTION('',(0.,1.,0.));
#6814=DIRECTION('',(0.,0.,1.));
#6815=DIRECTION('',(0.,1.,0.));
#6816=DIRECTION('',(0.,0.,1.));
#6817=DIRECTION('',(0.,1.,0.));
#6818=DIRECTION('',(0.,0.,1.));
#6819=DIRECTION('',(0.,1.,0.));
#6820=DIRECTION('',(0.,0.,1.));
#6821=DIRECTION('',(0.,1.,0.));
#6822=DIRECTION('',(0.,0.,1.));
#6823=DIRECTION('',(0.,1.,0.));
#6824=DIRECTION('',(0.,0.,1.));
#6825=DIRECTION('',(0.,1.,0.));
#6826=DIRECTION('',(0.,0.,1.));
#6827=DIRECTION('',(0.,1.,0.));
#6828=DIRECTION('',(0.,0.,1.));
#6829=DIRECTION('',(0.,1.,0.));
#6830=DIRECTION('',(0.,0.,1.));
#6831=DIRECTION('',(0.,1.,0.));
#6832=DIRECTION('',(0.,0.,1.));
#6833=DIRECTION('',(0.,1.,0.));
#6834=DIRECTION('',(0.,0.,1.));
#6835=DIRECTION('',(0.,1.,0.));
#6836=DIRECTION('',(0.,0.,1.));
#6837=DIRECTION('',(0.,1.,0.));
#6838=DIRECTION('',(0.,0.,1.));
#6839=DIRECTION('',(0.,1.,0.));
#6840=DIRECTION('',(0.,0.,1.));
#6841=DIRECTION('',(0.,1.,0.));
#6842=DIRECTION('',(0.,0.,1.));
#6843=DIRECTION('',(0.,1.,0.));
#6844=DIRECTION('',(0.,0.,1.));
#6845=DIRECTION('',(1.,0.,0.));
#6846=DIRECTION('',(0.,1.,0.));
#6847=DIRECTION('',(0.,0.,1.));
#6848=DIRECTION('',(-1.,0.,0.));
#6849=DIRECTION('',(0.5,0.,-0.866025403784439));
#6850=DIRECTION('',(-0.866025403784439,0.,-0.5));
#6851=DIRECTION('',(0.,-1.,0.));
#6852=DIRECTION('',(0.,-1.,0.));
#6853=DIRECTION('',(0.,0.,-1.));
#6854=DIRECTION('',(0.,-1.,0.));
#6855=DIRECTION('',(0.,-1.,0.));
#6856=DIRECTION('',(0.,0.,-1.));
#6857=DIRECTION('',(0.,-1.,0.));
#6858=DIRECTION('',(0.,0.,1.));
#6859=DIRECTION('',(1.,0.,0.));
#6860=DIRECTION('',(0.,-1.,0.));
#6861=DIRECTION('',(0.,-1.,0.));
#6862=DIRECTION('',(0.,0.,-1.));
#6863=DIRECTION('',(0.,-1.,0.));
#6864=DIRECTION('',(-1.91967175081904E-16,0.,-1.));
#6865=DIRECTION('',(-1.,0.,1.91967175081904E-16));
#6866=DIRECTION('',(0.,-1.,0.));
#6867=DIRECTION('',(0.,-1.,0.));
#6868=DIRECTION('',(0.,0.,-1.));
#6869=DIRECTION('',(0.,-1.,0.));
#6870=DIRECTION('',(0.,0.,-1.));
#6871=DIRECTION('',(0.,-1.,0.));
#6872=DIRECTION('',(0.,-1.,0.));
#6873=DIRECTION('',(0.,0.,-1.));
#6874=DIRECTION('',(-1.,0.,0.));
#6875=DIRECTION('',(0.,-1.,0.));
#6876=DIRECTION('',(0.,-1.,0.));
#6877=DIRECTION('',(0.,0.,-1.));
#6878=DIRECTION('',(0.,-1.,0.));
#6879=DIRECTION('',(0.,0.,1.));
#6880=DIRECTION('',(1.,0.,0.));
#6881=DIRECTION('',(0.,-1.,0.));
#6882=DIRECTION('',(0.,0.,-1.));
#6883=DIRECTION('',(-1.21904419394898E-29,-1.,3.49148133884314E-15));
#6884=DIRECTION('',(-1.21904419394898E-29,-1.,3.49148133884314E-15));
#6885=DIRECTION('',(0.,-1.,0.));
#6886=DIRECTION('',(0.,0.,-1.));
#6887=DIRECTION('',(-1.21904419394898E-29,-1.,3.49148133884314E-15));
#6888=DIRECTION('',(-1.21904419394898E-29,-1.,3.49148133884314E-15));
#6889=DIRECTION('',(0.,-1.,0.));
#6890=DIRECTION('',(0.,0.,-1.));
#6891=DIRECTION('',(-1.21904419394898E-29,-1.,3.49148133884314E-15));
#6892=DIRECTION('',(-1.21904419394898E-29,-1.,3.49148133884314E-15));
#6893=DIRECTION('',(0.,-1.,0.));
#6894=DIRECTION('',(0.,0.,-1.));
#6895=DIRECTION('',(-1.21904419394898E-29,-1.,3.49148133884314E-15));
#6896=DIRECTION('',(-1.21904419394898E-29,-1.,3.49148133884314E-15));
#6897=DIRECTION('',(0.,-1.,0.));
#6898=DIRECTION('',(0.,0.,-1.));
#6899=DIRECTION('',(-1.21904419394898E-29,-1.,3.49148133884314E-15));
#6900=DIRECTION('',(-1.21904419394898E-29,-1.,3.49148133884314E-15));
#6901=DIRECTION('',(0.,-1.,0.));
#6902=DIRECTION('',(0.,0.,-1.));
#6903=DIRECTION('',(-1.21904419394898E-29,-1.,3.49148133884314E-15));
#6904=DIRECTION('',(-1.21904419394898E-29,-1.,3.49148133884314E-15));
#6905=DIRECTION('',(0.,-1.,0.));
#6906=DIRECTION('',(0.,0.,-1.));
#6907=DIRECTION('',(-1.21904419394898E-29,-1.,3.49148133884314E-15));
#6908=DIRECTION('',(-1.21904419394898E-29,-1.,3.49148133884314E-15));
#6909=DIRECTION('',(0.,-1.,0.));
#6910=DIRECTION('',(0.,0.,-1.));
#6911=DIRECTION('',(-1.21904419394898E-29,-1.,3.49148133884314E-15));
#6912=DIRECTION('',(-1.21904419394898E-29,-1.,3.49148133884314E-15));
#6913=DIRECTION('',(0.,-1.,0.));
#6914=DIRECTION('',(0.,0.,-1.));
#6915=DIRECTION('',(-1.21904419394898E-29,-1.,3.49148133884314E-15));
#6916=DIRECTION('',(-1.21904419394898E-29,-1.,3.49148133884314E-15));
#6917=DIRECTION('',(0.,-1.,0.));
#6918=DIRECTION('',(0.,0.,-1.));
#6919=DIRECTION('',(-1.21904419394898E-29,-1.,3.49148133884314E-15));
#6920=DIRECTION('',(-1.21904419394898E-29,-1.,3.49148133884314E-15));
#6921=DIRECTION('',(-1.21904419394898E-29,-1.,3.49148133884314E-15));
#6922=DIRECTION('',(-1.,0.,-3.49148133884314E-15));
#6923=DIRECTION('',(-1.21904419394898E-29,-1.,3.49148133884314E-15));
#6924=DIRECTION('',(-1.21904419394898E-29,-1.,3.49148133884314E-15));
#6925=DIRECTION('',(-1.,0.,-3.49148133884314E-15));
#6926=DIRECTION('',(-1.21904419394898E-29,-1.,3.49148133884314E-15));
#6927=DIRECTION('',(-1.21904419394898E-29,-1.,3.49148133884314E-15));
#6928=DIRECTION('',(-1.,0.,-3.49148133884314E-15));
#6929=DIRECTION('',(-1.21904419394898E-29,-1.,3.49148133884314E-15));
#6930=DIRECTION('',(-1.,0.,-3.49148133884314E-15));
#6931=DIRECTION('',(-1.21904419394898E-29,-1.,3.49148133884314E-15));
#6932=DIRECTION('',(-1.21904419394898E-29,-1.,3.49148133884314E-15));
#6933=DIRECTION('',(-1.,0.,-3.49148133884314E-15));
#6934=DIRECTION('',(-1.21904419394898E-29,-1.,3.49148133884314E-15));
#6935=DIRECTION('',(-1.21904419394898E-29,-1.,3.49148133884314E-15));
#6936=DIRECTION('',(-1.,0.,-3.49148133884314E-15));
#6937=DIRECTION('',(-1.21904419394898E-29,-1.,3.49148133884314E-15));
#6938=DIRECTION('',(-1.,0.,-3.49148133884314E-15));
#6939=DIRECTION('',(-1.21904419394898E-29,-1.,3.49148133884314E-15));
#6940=DIRECTION('',(-1.21904419394898E-29,-1.,3.49148133884314E-15));
#6941=DIRECTION('',(-1.,0.,-3.49148133884314E-15));
#6942=DIRECTION('',(-1.21904419394898E-29,-1.,3.49148133884314E-15));
#6943=DIRECTION('',(-1.21904419394898E-29,-1.,3.49148133884314E-15));
#6944=DIRECTION('',(-1.,0.,-3.49148133884314E-15));
#6945=DIRECTION('',(-1.21904419394898E-29,-1.,3.49148133884314E-15));
#6946=DIRECTION('',(-1.,0.,-3.49148133884314E-15));
#6947=DIRECTION('',(-1.21904419394898E-29,-1.,3.49148133884314E-15));
#6948=DIRECTION('',(-1.21904419394898E-29,-1.,3.49148133884314E-15));
#6949=DIRECTION('',(-1.,0.,-3.49148133884314E-15));
#6950=DIRECTION('',(-1.21904419394898E-29,-1.,3.49148133884314E-15));
#6951=DIRECTION('',(-1.21904419394898E-29,-1.,3.49148133884314E-15));
#6952=DIRECTION('',(-1.,0.,-3.49148133884314E-15));
#6953=DIRECTION('',(-1.21904419394898E-29,-1.,3.49148133884314E-15));
#6954=DIRECTION('',(-1.,0.,-3.49148133884314E-15));
#6955=DIRECTION('',(-1.21904419394898E-29,-1.,3.49148133884314E-15));
#6956=DIRECTION('',(-1.21904419394898E-29,-1.,3.49148133884314E-15));
#6957=DIRECTION('',(-1.,0.,-3.49148133884314E-15));
#6958=DIRECTION('',(-1.21904419394898E-29,-1.,3.49148133884314E-15));
#6959=DIRECTION('',(-1.21904419394898E-29,-1.,3.49148133884314E-15));
#6960=DIRECTION('',(-1.,0.,-3.49148133884314E-15));
#6961=DIRECTION('',(-1.21904419394898E-29,-1.,3.49148133884314E-15));
#6962=DIRECTION('',(-1.,0.,-3.49148133884314E-15));
#6963=DIRECTION('',(-1.21904419394898E-29,-1.,3.49148133884314E-15));
#6964=DIRECTION('',(-1.21904419394898E-29,-1.,3.49148133884314E-15));
#6965=DIRECTION('',(-1.,0.,-3.49148133884314E-15));
#6966=DIRECTION('',(-1.21904419394898E-29,-1.,3.49148133884314E-15));
#6967=DIRECTION('',(-1.21904419394898E-29,-1.,3.49148133884314E-15));
#6968=DIRECTION('',(-1.,0.,-3.49148133884314E-15));
#6969=DIRECTION('',(-1.21904419394898E-29,-1.,3.49148133884314E-15));
#6970=DIRECTION('',(-1.,0.,-3.49148133884314E-15));
#6971=DIRECTION('',(-1.21904419394898E-29,-1.,3.49148133884314E-15));
#6972=DIRECTION('',(-1.21904419394898E-29,-1.,3.49148133884314E-15));
#6973=DIRECTION('',(-1.,0.,-3.49148133884314E-15));
#6974=DIRECTION('',(-1.21904419394898E-29,-1.,3.49148133884314E-15));
#6975=DIRECTION('',(-1.21904419394898E-29,-1.,3.49148133884314E-15));
#6976=DIRECTION('',(-1.,0.,-3.49148133884314E-15));
#6977=DIRECTION('',(-1.21904419394898E-29,-1.,3.49148133884314E-15));
#6978=DIRECTION('',(-1.,0.,-3.49148133884314E-15));
#6979=DIRECTION('',(-1.21904419394898E-29,-1.,3.49148133884314E-15));
#6980=DIRECTION('',(-1.21904419394898E-29,-1.,3.49148133884314E-15));
#6981=DIRECTION('',(-1.,0.,-3.49148133884314E-15));
#6982=DIRECTION('',(-1.21904419394898E-29,-1.,3.49148133884314E-15));
#6983=DIRECTION('',(-1.21904419394898E-29,-1.,3.49148133884314E-15));
#6984=DIRECTION('',(-1.,0.,-3.49148133884314E-15));
#6985=DIRECTION('',(-1.21904419394898E-29,-1.,3.49148133884314E-15));
#6986=DIRECTION('',(-1.,0.,-3.49148133884314E-15));
#6987=DIRECTION('',(-1.21904419394898E-29,-1.,3.49148133884314E-15));
#6988=DIRECTION('',(-1.21904419394898E-29,-1.,3.49148133884314E-15));
#6989=DIRECTION('',(-1.,0.,-3.49148133884314E-15));
#6990=DIRECTION('',(-1.21904419394898E-29,-1.,3.49148133884314E-15));
#6991=DIRECTION('',(-1.21904419394898E-29,-1.,3.49148133884314E-15));
#6992=DIRECTION('',(-1.,0.,-3.49148133884314E-15));
#6993=DIRECTION('',(-1.21904419394898E-29,-1.,3.49148133884314E-15));
#6994=DIRECTION('',(-1.,0.,-3.49148133884314E-15));
#6995=DIRECTION('',(-1.21904419394898E-29,-1.,3.49148133884314E-15));
#6996=DIRECTION('',(-1.21904419394898E-29,-1.,3.49148133884314E-15));
#6997=DIRECTION('',(-1.,0.,-3.49148133884314E-15));
#6998=DIRECTION('',(-1.21904419394898E-29,-1.,3.49148133884314E-15));
#6999=DIRECTION('',(-1.21904419394898E-29,-1.,3.49148133884314E-15));
#7000=DIRECTION('',(-1.,0.,-3.49148133884314E-15));
#7001=DIRECTION('',(-1.21904419394898E-29,-1.,3.49148133884314E-15));
#7002=DIRECTION('',(-1.,0.,-3.49148133884314E-15));
#7003=DIRECTION('',(-1.21904419394898E-29,-1.,3.49148133884314E-15));
#7004=DIRECTION('',(-1.21904419394898E-29,-1.,3.49148133884314E-15));
#7005=DIRECTION('',(-1.,0.,-3.49148133884314E-15));
#7006=DIRECTION('',(-1.21904419394898E-29,-1.,3.49148133884314E-15));
#7007=DIRECTION('',(-1.21904419394898E-29,-1.,3.49148133884314E-15));
#7008=DIRECTION('',(-1.,0.,-3.49148133884314E-15));
#7009=DIRECTION('',(0.298895772662389,-0.95428576280093,-2.96912440601756E-16));
#7010=DIRECTION('',(-0.95428576280093,-0.298895772662389,-1.16456820595263E-16));
#7011=DIRECTION('',(1.1395736960892E-16,-9.24063370720862E-17,1.));
#7012=DIRECTION('',(-0.156844626527356,0.987623290090657,1.09136251720711E-16));
#7013=DIRECTION('',(-1.,0.,0.));
#7014=DIRECTION('',(0.,0.,1.));
#7015=DIRECTION('',(0.,-1.,0.));
#7016=DIRECTION('',(0.,0.,-1.));
#7017=DIRECTION('',(0.,-1.,0.));
#7018=DIRECTION('',(0.,0.,-1.));
#7019=DIRECTION('',(-1.,0.,0.));
#7020=DIRECTION('',(0.,0.,1.));
#7021=DIRECTION('',(0.,-1.,0.));
#7022=DIRECTION('',(0.,0.,1.));
#7023=DIRECTION('',(0.,-1.,0.));
#7024=DIRECTION('',(0.,0.,-1.));
#7025=DIRECTION('',(0.,0.,-1.));
#7026=DIRECTION('',(0.,0.,-1.));
#7027=DIRECTION('',(-1.,0.,0.));
#7028=DIRECTION('',(1.,0.,0.));
#7029=DIRECTION('',(0.,-1.,0.));
#7030=DIRECTION('',(0.,0.,1.));
#7031=DIRECTION('',(1.,0.,0.));
#7032=DIRECTION('',(-1.,-3.46944695195362E-16,0.));
#7033=DIRECTION('',(0.,0.,1.));
#7034=DIRECTION('',(1.,0.,0.));
#7035=DIRECTION('',(0.,-1.,0.));
#7036=DIRECTION('',(0.,0.,-1.));
#7037=DIRECTION('',(-1.,0.,0.));
#7038=DIRECTION('',(-1.,0.,0.));
#7039=DIRECTION('',(0.,-1.,0.));
#7040=DIRECTION('',(1.,0.,0.));
#7041=DIRECTION('',(1.,0.,0.));
#7042=DIRECTION('',(0.,-1.,0.));
#7043=DIRECTION('',(-1.,0.,0.));
#7044=DIRECTION('',(0.,0.,1.));
#7045=DIRECTION('',(0.,0.,-1.));
#7046=DIRECTION('',(0.,-1.,0.));
#7047=DIRECTION('',(0.,0.,-1.));
#7048=DIRECTION('',(0.,-1.,0.));
#7049=DIRECTION('',(-1.,0.,0.));
#7050=DIRECTION('',(0.,0.,1.));
#7051=DIRECTION('',(0.,0.,1.));
#7052=DIRECTION('',(0.,-1.,0.));
#7053=DIRECTION('',(0.,0.,-1.));
#7054=DIRECTION('',(0.,0.,-1.));
#7055=DIRECTION('',(0.,-1.,0.));
#7056=DIRECTION('',(0.,0.,-1.));
#7057=DIRECTION('',(-1.,0.,0.));
#7058=DIRECTION('',(0.,-1.,0.));
#7059=DIRECTION('',(1.,0.,0.));
#7060=DIRECTION('',(0.,-1.,0.));
#7061=DIRECTION('',(1.,0.,0.));
#7062=DIRECTION('',(0.,0.,-1.));
#7063=DIRECTION('',(-1.,0.,0.));
#7064=DIRECTION('',(0.,-1.,0.));
#7065=DIRECTION('',(-1.,0.,0.));
#7066=DIRECTION('',(0.,-1.,0.));
#7067=DIRECTION('',(1.,0.,0.));
#7068=DIRECTION('',(1.,0.,0.));
#7069=DIRECTION('',(0.,1.,0.));
#7070=DIRECTION('',(0.,0.,1.));
#7071=DIRECTION('',(0.,1.,0.));
#7072=DIRECTION('',(0.,0.,1.));
#7073=DIRECTION('',(0.,-1.,0.));
#7074=DIRECTION('',(0.,0.,-1.));
#7075=DIRECTION('',(0.,-1.,0.));
#7076=DIRECTION('',(0.,1.,0.));
#7077=DIRECTION('',(0.,0.,1.));
#7078=DIRECTION('',(0.,-1.,0.));
#7079=DIRECTION('',(0.,0.,-1.));
#7080=DIRECTION('',(0.,-1.,0.));
#7081=DIRECTION('',(0.,0.,-1.));
#7082=DIRECTION('',(0.,-1.,0.));
#7083=DIRECTION('',(0.,0.,-1.));
#7084=DIRECTION('',(0.,1.,0.));
#7085=DIRECTION('',(0.,0.,1.));
#7086=DIRECTION('',(0.,-1.,0.));
#7087=DIRECTION('',(0.,0.,-1.));
#7088=DIRECTION('',(0.,-1.,0.));
#7089=DIRECTION('',(0.,0.,-1.));
#7090=DIRECTION('',(0.,-1.,0.));
#7091=DIRECTION('',(0.,0.,-1.));
#7092=DIRECTION('',(0.,-1.,0.));
#7093=DIRECTION('',(0.,0.,-1.));
#7094=DIRECTION('',(0.,1.,0.));
#7095=DIRECTION('',(0.,0.,1.));
#7096=DIRECTION('',(0.,1.,0.));
#7097=DIRECTION('',(0.,0.,1.));
#7098=DIRECTION('',(0.,-1.,0.));
#7099=DIRECTION('',(0.,0.,-1.));
#7100=DIRECTION('',(0.,1.,0.));
#7101=DIRECTION('',(0.,0.,1.));
#7102=DIRECTION('',(0.,-1.,0.));
#7103=DIRECTION('',(0.,0.,-1.));
#7104=DIRECTION('',(0.,-1.,0.));
#7105=DIRECTION('',(0.,0.,-1.));
#7106=DIRECTION('',(0.,-1.,0.));
#7107=DIRECTION('',(0.,0.,-1.));
#7108=DIRECTION('',(0.,1.,0.));
#7109=DIRECTION('',(0.,0.,1.));
#7110=DIRECTION('',(0.,-1.,0.));
#7111=DIRECTION('',(0.,-1.,0.));
#7112=DIRECTION('',(0.,0.,-1.));
#7113=DIRECTION('',(0.,-1.,0.));
#7114=DIRECTION('',(0.,0.,-1.));
#7115=DIRECTION('',(0.,-1.,0.));
#7116=DIRECTION('',(0.,0.,-1.));
#7117=DIRECTION('',(0.,-1.,0.));
#7118=DIRECTION('',(0.,0.,-1.));
#7119=DIRECTION('',(0.,0.,-1.));
#7120=DIRECTION('',(-1.,0.,0.));
#7121=DIRECTION('',(1.,0.,0.));
#7122=DIRECTION('',(0.,0.,1.));
#7123=DIRECTION('',(1.,0.,0.));
#7124=DIRECTION('',(1.,-3.46944695195362E-16,0.));
#7125=DIRECTION('',(0.,0.,1.));
#7126=DIRECTION('',(1.,0.,0.));
#7127=DIRECTION('',(0.,-1.,0.));
#7128=DIRECTION('',(0.,0.,-1.));
#7129=DIRECTION('',(0.,-1.,0.));
#7130=DIRECTION('',(0.,0.,-1.));
#7131=DIRECTION('',(0.,-1.,0.));
#7132=DIRECTION('',(0.,0.,-1.));
#7133=DIRECTION('',(0.,-1.,0.));
#7134=DIRECTION('',(0.,0.,-1.));
#7135=DIRECTION('',(0.,-1.,0.));
#7136=DIRECTION('',(0.,0.,-1.));
#7137=DIRECTION('',(0.,-1.,0.));
#7138=DIRECTION('',(0.,0.,-1.));
#7139=DIRECTION('',(0.,1.,0.));
#7140=DIRECTION('',(0.,0.,1.));
#7141=DIRECTION('',(-1.,0.,0.));
#7142=DIRECTION('',(0.,1.,0.));
#7143=DIRECTION('',(0.,0.,1.));
#7144=DIRECTION('',(-1.,0.,0.));
#7145=DIRECTION('',(0.,0.,1.));
#7146=DIRECTION('',(0.,-1.,0.));
#7147=DIRECTION('',(0.,0.,-1.));
#7148=DIRECTION('',(0.,-1.,0.));
#7149=DIRECTION('',(0.,0.,-1.));
#7150=DIRECTION('',(0.,-1.,0.));
#7151=DIRECTION('',(0.,0.,-1.));
#7152=DIRECTION('',(0.,-1.,0.));
#7153=DIRECTION('',(0.,0.,-1.));
#7154=DIRECTION('',(0.,-1.,0.));
#7155=DIRECTION('',(0.,0.,-1.));
#7156=DIRECTION('',(0.,1.,0.));
#7157=DIRECTION('',(0.,0.,1.));
#7158=DIRECTION('',(0.,1.,0.));
#7159=DIRECTION('',(0.,0.,1.));
#7160=DIRECTION('',(0.,1.,0.));
#7161=DIRECTION('',(0.,0.,1.));
#7162=DIRECTION('',(0.,1.,0.));
#7163=DIRECTION('',(0.,0.,1.));
#7164=DIRECTION('',(0.,-1.,0.));
#7165=DIRECTION('',(0.,0.,-1.));
#7166=DIRECTION('',(0.,0.,1.));
#7167=DIRECTION('',(1.,0.,0.));
#7168=DIRECTION('',(0.,0.,1.));
#7169=DIRECTION('',(0.,0.,1.));
#7170=DIRECTION('',(1.,0.,0.));
#7171=DIRECTION('',(0.,0.,1.));
#7172=DIRECTION('',(-3.46944695195362E-16,1.,0.));
#7173=DIRECTION('',(-1.,-3.46944695195362E-16,0.));
#7174=DIRECTION('',(-1.,-3.46944695195362E-16,0.));
#7175=DIRECTION('',(-3.46944695195362E-16,1.,0.));
#7176=DIRECTION('',(-1.,-3.46944695195362E-16,0.));
#7177=DIRECTION('',(-1.,-3.46944695195362E-16,0.));
#7178=DIRECTION('',(0.,0.,1.));
#7179=DIRECTION('',(0.,0.,1.));
#7180=DIRECTION('',(1.,0.,0.));
#7181=DIRECTION('',(0.,0.,1.));
#7182=DIRECTION('',(1.,0.,0.));
#7183=DIRECTION('',(0.,0.,1.));
#7184=DIRECTION('',(-3.46944695195362E-16,-1.,0.));
#7185=DIRECTION('',(1.,-3.46944695195362E-16,0.));
#7186=DIRECTION('',(1.,-3.46944695195362E-16,0.));
#7187=DIRECTION('',(0.,0.,1.));
#7188=DIRECTION('',(1.,0.,0.));
#7189=DIRECTION('',(0.,1.,0.));
#7190=DIRECTION('',(0.,0.,1.));
#7191=DIRECTION('',(1.,0.,0.));
#7192=DIRECTION('',(1.,0.,0.));
#7193=DIRECTION('',(0.,0.,1.));
#7194=DIRECTION('',(1.,0.,0.));
#7195=DIRECTION('',(-1.,0.,0.));
#7196=DIRECTION('',(0.,1.,0.));
#7197=DIRECTION('',(0.,0.,1.));
#7198=DIRECTION('',(1.,0.,0.));
#7199=DIRECTION('',(0.,0.,1.));
#7200=DIRECTION('',(0.,0.,1.));
#7201=DIRECTION('',(1.,0.,0.));
#7202=DIRECTION('',(0.,0.,1.));
#7203=DIRECTION('',(0.,1.,0.));
#7204=DIRECTION('',(0.,0.,1.));
#7205=DIRECTION('',(-1.,0.,0.));
#7206=DIRECTION('',(0.,1.,0.));
#7207=DIRECTION('',(0.,0.,1.));
#7208=DIRECTION('',(0.,0.,1.));
#7209=DIRECTION('',(1.,0.,0.));
#7210=DIRECTION('',(0.,0.,1.));
#7211=DIRECTION('',(1.,0.,0.));
#7212=DIRECTION('',(0.,0.,1.));
#7213=DIRECTION('',(0.,-1.,0.));
#7214=DIRECTION('',(0.,0.,-1.));
#7215=DIRECTION('',(1.,0.,0.));
#7216=DIRECTION('',(0.,0.,1.));
#7217=DIRECTION('',(1.,0.,0.));
#7218=DIRECTION('',(0.,1.,0.));
#7219=DIRECTION('',(0.,0.,1.));
#7220=DIRECTION('',(0.,-1.,0.));
#7221=DIRECTION('',(0.,0.,-1.));
#7222=DIRECTION('',(0.,1.,0.));
#7223=DIRECTION('',(0.,0.,1.));
#7224=DIRECTION('',(0.,1.,0.));
#7225=DIRECTION('',(0.,0.,1.));
#7226=DIRECTION('',(0.,1.,0.));
#7227=DIRECTION('',(0.,0.,1.));
#7228=DIRECTION('',(0.,1.,0.));
#7229=DIRECTION('',(0.,0.,1.));
#7230=DIRECTION('',(0.,-1.,0.));
#7231=DIRECTION('',(0.,0.,-1.));
#7232=DIRECTION('',(0.980746659781992,0.195284380651566,-2.45110728784917E-17));
#7233=DIRECTION('',(2.7755575615629E-17,-1.38777878078145E-17,1.));
#7234=DIRECTION('',(0.,1.,0.));
#7235=DIRECTION('',(0.,0.,1.));
#7236=DIRECTION('',(0.,1.,0.));
#7237=DIRECTION('',(1.,0.,0.));
#7238=DIRECTION('',(0.,1.,0.));
#7239=DIRECTION('',(1.,0.,0.));
#7240=DIRECTION('',(0.,1.,0.));
#7241=DIRECTION('',(0.,0.,1.));
#7242=DIRECTION('',(0.866025403784438,0.,0.5));
#7243=DIRECTION('',(0.,1.,0.));
#7244=DIRECTION('',(0.,0.,1.));
#7245=DIRECTION('',(-0.866025403784438,0.,-0.5));
#7246=DIRECTION('',(0.,1.,0.));
#7247=DIRECTION('',(0.,0.,1.));
#7248=DIRECTION('',(0.,1.,0.));
#7249=DIRECTION('',(0.,0.,1.));
#7250=DIRECTION('',(0.,1.,0.));
#7251=DIRECTION('',(0.,0.,1.));
#7252=DIRECTION('',(-0.866025403784438,0.,-0.5));
#7253=DIRECTION('',(0.,1.,0.));
#7254=DIRECTION('',(0.,0.,1.));
#7255=DIRECTION('',(0.866025403784438,0.,0.5));
#7256=DIRECTION('',(0.,1.,0.));
#7257=DIRECTION('',(0.,0.,1.));
#7258=DIRECTION('',(0.,-1.,0.));
#7259=DIRECTION('',(0.,0.,-1.));
#7260=DIRECTION('',(0.,-1.,0.));
#7261=DIRECTION('',(0.,-1.,0.));
#7262=DIRECTION('',(0.5,0.,-0.866025403784438));
#7263=DIRECTION('',(-0.866025403784438,0.,-0.5));
#7264=DIRECTION('',(0.,-1.,0.));
#7265=DIRECTION('',(0.,-1.,0.));
#7266=DIRECTION('',(0.,0.,-1.));
#7267=DIRECTION('',(0.,-1.,0.));
#7268=DIRECTION('',(-0.5,0.,0.866025403784438));
#7269=DIRECTION('',(0.866025403784438,0.,0.5));
#7270=DIRECTION('',(0.,-1.,0.));
#7271=DIRECTION('',(0.,0.,-1.));
#7272=DIRECTION('',(0.,1.,0.));
#7273=DIRECTION('',(0.,0.,1.));
#7274=DIRECTION('',(0.,1.,0.));
#7275=DIRECTION('',(1.,0.,0.));
#7276=DIRECTION('',(0.,1.,0.));
#7277=DIRECTION('',(0.,0.,1.));
#7278=DIRECTION('',(0.,-1.,0.));
#7279=DIRECTION('',(0.,0.,-1.));
#7280=DIRECTION('',(0.,-1.,0.));
#7281=DIRECTION('',(0.,0.,-1.));
#7282=DIRECTION('',(0.,1.,0.));
#7283=DIRECTION('',(0.,0.,1.));
#7284=DIRECTION('',(0.,1.,0.));
#7285=DIRECTION('',(0.,0.,1.));
#7286=DIRECTION('',(0.,1.,0.));
#7287=DIRECTION('',(0.,0.,1.));
#7288=DIRECTION('',(0.,1.,0.));
#7289=DIRECTION('',(1.,0.,0.));
#7290=DIRECTION('',(0.,1.,0.));
#7291=DIRECTION('',(0.,0.,1.));
#7292=DIRECTION('',(0.,-1.,0.));
#7293=DIRECTION('',(0.,0.,-1.));
#7294=DIRECTION('',(0.,-1.,0.));
#7295=DIRECTION('',(0.,0.,-1.));
#7296=DIRECTION('',(0.,1.,0.));
#7297=DIRECTION('',(0.,0.,1.));
#7298=DIRECTION('',(0.,1.,0.));
#7299=DIRECTION('',(0.,0.,1.));
#7300=DIRECTION('',(-0.987623290090657,-0.156844626527356,-9.0143056710024E-17));
#7301=DIRECTION('',(0.156844626527356,-0.987623290090657,-3.26262653247095E-16));
#7302=DIRECTION('',(-0.866025403784439,0.,-0.5));
#7303=DIRECTION('',(-0.5,0.,0.866025403784439));
#7304=DIRECTION('',(0.5,0.,-0.866025403784439));
#7305=DIRECTION('',(0.,-1.,0.));
#7306=DIRECTION('',(0.5,0.,-0.866025403784439));
#7307=DIRECTION('',(0.,-1.,0.));
#7308=DIRECTION('',(0.5,0.,-0.866025403784439));
#7309=DIRECTION('',(-0.866025403784439,0.,-0.5));
#7310=DIRECTION('',(0.866025403784439,0.,0.5));
#7311=DIRECTION('',(0.,-1.,0.));
#7312=DIRECTION('',(0.866025403784439,0.,0.5));
#7313=DIRECTION('',(-0.866025403784434,0.,-0.500000000000008));
#7314=DIRECTION('',(-0.500000000000009,0.,0.866025403784434));
#7315=DIRECTION('',(0.500000000000009,0.,-0.866025403784434));
#7316=DIRECTION('',(0.,-1.,0.));
#7317=DIRECTION('',(0.500000000000009,0.,-0.866025403784434));
#7318=DIRECTION('',(0.,-1.,0.));
#7319=DIRECTION('',(0.,0.,-1.));
#7320=DIRECTION('',(0.,-1.,0.));
#7321=DIRECTION('',(0.,0.,-1.));
#7322=DIRECTION('',(0.,-1.,0.));
#7323=DIRECTION('',(0.,0.,-1.));
#7324=DIRECTION('',(0.500000000000008,0.,-0.866025403784434));
#7325=DIRECTION('',(-0.866025403784434,0.,-0.500000000000009));
#7326=DIRECTION('',(0.866025403784434,0.,0.500000000000009));
#7327=DIRECTION('',(0.866025403784434,0.,0.500000000000009));
#7328=DIRECTION('',(0.,-1.,0.));
#7329=DIRECTION('',(0.,0.,-1.));
#7330=DIRECTION('',(0.,-1.,0.));
#7331=DIRECTION('',(0.,0.,-1.));
#7332=DIRECTION('',(0.,-1.,0.));
#7333=DIRECTION('',(0.,0.,-1.));
#7334=DIRECTION('',(0.,-1.,0.));
#7335=DIRECTION('',(0.,0.,-1.));
#7336=DIRECTION('',(0.,-1.,0.));
#7337=DIRECTION('',(0.,0.,-1.));
#7338=DIRECTION('',(0.,-1.,0.));
#7339=DIRECTION('',(0.,0.,-1.));
#7340=DIRECTION('',(0.,-1.,0.));
#7341=DIRECTION('',(0.,0.,-1.));
#7342=DIRECTION('',(0.,-1.,0.));
#7343=DIRECTION('',(0.,0.,-1.));
#7344=DIRECTION('',(0.,-1.,0.));
#7345=DIRECTION('',(0.,0.,-1.));
#7346=DIRECTION('',(0.,-1.,0.));
#7347=DIRECTION('',(0.,0.,-1.));
#7348=DIRECTION('',(0.,-1.,0.));
#7349=DIRECTION('',(0.,0.,-1.));
#7350=DIRECTION('',(0.,-1.,0.));
#7351=DIRECTION('',(0.,0.,-1.));
#7352=DIRECTION('',(0.,-1.,0.));
#7353=DIRECTION('',(0.,0.,-1.));
#7354=DIRECTION('',(0.,-1.,0.));
#7355=DIRECTION('',(0.,0.,-1.));
#7356=DIRECTION('',(0.,-1.,0.));
#7357=DIRECTION('',(0.,0.,-1.));
#7358=DIRECTION('',(0.,-1.,0.));
#7359=DIRECTION('',(0.,0.,-1.));
#7360=DIRECTION('',(0.,1.,0.));
#7361=DIRECTION('',(0.,0.,1.));
#7362=DIRECTION('',(0.987717584236107,0.156249716130265,-5.0912723267111E-17));
#7363=DIRECTION('',(-0.156249716130265,0.987717584236107,7.00546385119699E-17));
#7364=DIRECTION('',(0.,1.,0.));
#7365=DIRECTION('',(0.,0.,1.));
#7366=DIRECTION('',(0.,1.,0.));
#7367=DIRECTION('',(-6.12323399573674E-17,0.,1.));
#7368=DIRECTION('',(0.,1.,0.));
#7369=DIRECTION('',(0.,0.,1.));
#7370=DIRECTION('',(0.,1.,0.));
#7371=DIRECTION('',(0.,0.,1.));
#7372=DIRECTION('',(0.,1.,0.));
#7373=DIRECTION('',(0.,0.,1.));
#7374=DIRECTION('',(0.,1.,0.));
#7375=DIRECTION('',(0.,0.,1.));
#7376=DIRECTION('',(0.,1.,0.));
#7377=DIRECTION('',(0.,0.,1.));
#7378=DIRECTION('',(0.,1.,0.));
#7379=DIRECTION('',(0.,0.,1.));
#7380=DIRECTION('',(0.,1.,0.));
#7381=DIRECTION('',(0.,0.,1.));
#7382=DIRECTION('',(0.,1.,0.));
#7383=DIRECTION('',(0.,0.,1.));
#7384=DIRECTION('',(0.,-1.,0.));
#7385=DIRECTION('',(0.,0.,-1.));
#7386=DIRECTION('',(0.,1.,0.));
#7387=DIRECTION('',(0.,0.,1.));
#7388=DIRECTION('',(0.,1.,0.));
#7389=DIRECTION('',(0.,0.,1.));
#7390=DIRECTION('',(0.,1.,0.));
#7391=DIRECTION('',(0.,0.,1.));
#7392=DIRECTION('',(0.999955147140781,0.00947120407651268,7.08546361463669E-16));
#7393=DIRECTION('',(-0.00947120407651268,0.999955147140781,-8.53381320735012E-16));
#7394=DIRECTION('',(-1.,0.,0.));
#7395=DIRECTION('',(0.,0.,1.));
#7396=DIRECTION('',(1.,0.,0.));
#7397=DIRECTION('',(0.,0.,-1.));
#7398=DIRECTION('',(1.,0.,0.));
#7399=DIRECTION('',(0.,0.,-1.));
#7400=DIRECTION('',(-1.,0.,0.));
#7401=DIRECTION('',(0.,0.,1.));
#7402=DIRECTION('',(-1.,0.,0.));
#7403=DIRECTION('',(0.,0.,1.));
#7404=DIRECTION('',(1.,0.,0.));
#7405=DIRECTION('',(0.,0.,-1.));
#7406=DIRECTION('',(-1.,0.,0.));
#7407=DIRECTION('',(0.,0.,1.));
#7408=DIRECTION('',(-1.,0.,0.));
#7409=DIRECTION('',(0.,0.989821441880932,0.142314838273289));
#7410=DIRECTION('',(-1.,0.,0.));
#7411=DIRECTION('',(0.,0.989821441880932,0.142314838273289));
#7412=DIRECTION('',(-1.,0.,0.));
#7413=DIRECTION('',(0.,0.989821441880932,0.142314838273289));
#7414=DIRECTION('',(-1.,0.,0.));
#7415=DIRECTION('',(0.,0.,1.));
#7416=DIRECTION('',(-1.,0.,0.));
#7417=DIRECTION('',(0.,0.909631995354517,0.41541501300189));
#7418=DIRECTION('',(-1.,0.,0.));
#7419=DIRECTION('',(0.,0.909631995354517,0.41541501300189));
#7420=DIRECTION('',(-1.,0.,0.));
#7421=DIRECTION('',(0.,0.909631995354517,0.41541501300189));
#7422=DIRECTION('',(-1.,0.,0.));
#7423=DIRECTION('',(0.,0.,1.));
#7424=DIRECTION('',(-1.,0.,0.));
#7425=DIRECTION('',(0.,0.755749574354255,0.654860733945289));
#7426=DIRECTION('',(-1.,0.,0.));
#7427=DIRECTION('',(0.,0.755749574354255,0.654860733945289));
#7428=DIRECTION('',(-1.,0.,0.));
#7429=DIRECTION('',(0.,0.755749574354255,0.654860733945289));
#7430=DIRECTION('',(-1.,0.,0.));
#7431=DIRECTION('',(0.,0.,1.));
#7432=DIRECTION('',(-1.,0.,0.));
#7433=DIRECTION('',(0.,0.540640817455593,0.841253532831184));
#7434=DIRECTION('',(-1.,0.,0.));
#7435=DIRECTION('',(0.,0.540640817455593,0.841253532831184));
#7436=DIRECTION('',(-1.,0.,0.));
#7437=DIRECTION('',(0.,0.540640817455593,0.841253532831184));
#7438=DIRECTION('',(-1.,0.,0.));
#7439=DIRECTION('',(0.,0.,1.));
#7440=DIRECTION('',(-1.,0.,0.));
#7441=DIRECTION('',(0.,0.281732556841424,0.959492973614499));
#7442=DIRECTION('',(-1.,0.,0.));
#7443=DIRECTION('',(0.,0.281732556841424,0.959492973614499));
#7444=DIRECTION('',(-1.,0.,0.));
#7445=DIRECTION('',(0.,0.281732556841424,0.959492973614499));
#7446=DIRECTION('',(-1.,0.,0.));
#7447=DIRECTION('',(0.,0.,1.));
#7448=DIRECTION('',(-1.,0.,0.));
#7449=DIRECTION('',(0.,-6.53887346783621E-15,1.));
#7450=DIRECTION('',(-1.,0.,0.));
#7451=DIRECTION('',(0.,-6.53887346783621E-15,1.));
#7452=DIRECTION('',(-1.,0.,0.));
#7453=DIRECTION('',(0.,-6.53887346783621E-15,1.));
#7454=DIRECTION('',(-1.,0.,0.));
#7455=DIRECTION('',(0.,0.,1.));
#7456=DIRECTION('',(-1.,0.,0.));
#7457=DIRECTION('',(0.,-0.281732556841436,0.959492973614495));
#7458=DIRECTION('',(-1.,0.,0.));
#7459=DIRECTION('',(0.,-0.281732556841436,0.959492973614495));
#7460=DIRECTION('',(-1.,0.,0.));
#7461=DIRECTION('',(0.,-0.281732556841436,0.959492973614495));
#7462=DIRECTION('',(-1.,0.,0.));
#7463=DIRECTION('',(0.,0.,1.));
#7464=DIRECTION('',(-1.,0.,0.));
#7465=DIRECTION('',(0.,-0.540640817455604,0.841253532831177));
#7466=DIRECTION('',(-1.,0.,0.));
#7467=DIRECTION('',(0.,-0.540640817455604,0.841253532831177));
#7468=DIRECTION('',(-1.,0.,0.));
#7469=DIRECTION('',(0.,-0.540640817455604,0.841253532831177));
#7470=DIRECTION('',(-1.,0.,0.));
#7471=DIRECTION('',(0.,0.,1.));
#7472=DIRECTION('',(-1.,0.,0.));
#7473=DIRECTION('',(0.,-0.755749574354264,0.654860733945279));
#7474=DIRECTION('',(-1.,0.,0.));
#7475=DIRECTION('',(0.,-0.755749574354264,0.654860733945279));
#7476=DIRECTION('',(-1.,0.,0.));
#7477=DIRECTION('',(0.,-0.755749574354264,0.654860733945279));
#7478=DIRECTION('',(-1.,0.,0.));
#7479=DIRECTION('',(0.,0.,1.));
#7480=DIRECTION('',(-1.,0.,0.));
#7481=DIRECTION('',(0.,-0.909631995354522,0.415415013001878));
#7482=DIRECTION('',(-1.,0.,0.));
#7483=DIRECTION('',(0.,-0.909631995354522,0.415415013001878));
#7484=DIRECTION('',(-1.,0.,0.));
#7485=DIRECTION('',(0.,-0.909631995354522,0.415415013001878));
#7486=DIRECTION('',(-1.,0.,0.));
#7487=DIRECTION('',(0.,0.,1.));
#7488=DIRECTION('',(-1.,0.,0.));
#7489=DIRECTION('',(0.,-0.989821441880934,0.142314838273276));
#7490=DIRECTION('',(-1.,0.,0.));
#7491=DIRECTION('',(0.,-0.989821441880934,0.142314838273276));
#7492=DIRECTION('',(-1.,0.,0.));
#7493=DIRECTION('',(0.,-0.989821441880934,0.142314838273276));
#7494=DIRECTION('',(-1.,0.,0.));
#7495=DIRECTION('',(0.,0.,1.));
#7496=DIRECTION('',(-1.,0.,0.));
#7497=DIRECTION('',(0.,-0.989821441880931,-0.142314838273295));
#7498=DIRECTION('',(-1.,0.,0.));
#7499=DIRECTION('',(0.,-0.989821441880931,-0.142314838273295));
#7500=DIRECTION('',(-1.,0.,0.));
#7501=DIRECTION('',(0.,-0.989821441880931,-0.142314838273295));
#7502=DIRECTION('',(-1.,0.,0.));
#7503=DIRECTION('',(0.,0.,1.));
#7504=DIRECTION('',(-1.,0.,0.));
#7505=DIRECTION('',(0.,-0.909631995354514,-0.415415013001896));
#7506=DIRECTION('',(-1.,0.,0.));
#7507=DIRECTION('',(0.,-0.909631995354514,-0.415415013001896));
#7508=DIRECTION('',(-1.,0.,0.));
#7509=DIRECTION('',(0.,-0.909631995354514,-0.415415013001896));
#7510=DIRECTION('',(-1.,0.,0.));
#7511=DIRECTION('',(0.,0.,1.));
#7512=DIRECTION('',(-1.,0.,0.));
#7513=DIRECTION('',(0.,-0.755749574354251,-0.654860733945294));
#7514=DIRECTION('',(-1.,0.,0.));
#7515=DIRECTION('',(0.,-0.755749574354251,-0.654860733945294));
#7516=DIRECTION('',(-1.,0.,0.));
#7517=DIRECTION('',(0.,-0.755749574354251,-0.654860733945294));
#7518=DIRECTION('',(-1.,0.,0.));
#7519=DIRECTION('',(0.,0.,1.));
#7520=DIRECTION('',(-1.,0.,0.));
#7521=DIRECTION('',(0.,-0.540640817455587,-0.841253532831188));
#7522=DIRECTION('',(-1.,0.,0.));
#7523=DIRECTION('',(0.,-0.540640817455587,-0.841253532831188));
#7524=DIRECTION('',(-1.,0.,0.));
#7525=DIRECTION('',(0.,-0.540640817455587,-0.841253532831188));
#7526=DIRECTION('',(-1.,0.,0.));
#7527=DIRECTION('',(0.,0.,1.));
#7528=DIRECTION('',(-1.,0.,0.));
#7529=DIRECTION('',(0.,-0.281732556841418,-0.959492973614501));
#7530=DIRECTION('',(-1.,0.,0.));
#7531=DIRECTION('',(0.,-0.281732556841418,-0.959492973614501));
#7532=DIRECTION('',(-1.,0.,0.));
#7533=DIRECTION('',(0.,-0.281732556841418,-0.959492973614501));
#7534=DIRECTION('',(-1.,0.,0.));
#7535=DIRECTION('',(0.,0.,1.));
#7536=DIRECTION('',(-1.,0.,0.));
#7537=DIRECTION('',(0.,0.,-1.));
#7538=DIRECTION('',(-1.,0.,0.));
#7539=DIRECTION('',(0.,0.,-1.));
#7540=DIRECTION('',(-1.,0.,0.));
#7541=DIRECTION('',(0.,0.,-1.));
#7542=DIRECTION('',(-1.,0.,0.));
#7543=DIRECTION('',(0.,0.,1.));
#7544=DIRECTION('',(-1.,0.,0.));
#7545=DIRECTION('',(0.,0.281732556841431,-0.959492973614497));
#7546=DIRECTION('',(-1.,0.,0.));
#7547=DIRECTION('',(0.,0.281732556841431,-0.959492973614497));
#7548=DIRECTION('',(-1.,0.,0.));
#7549=DIRECTION('',(0.,0.281732556841431,-0.959492973614497));
#7550=DIRECTION('',(-1.,0.,0.));
#7551=DIRECTION('',(0.,0.,1.));
#7552=DIRECTION('',(-1.,0.,0.));
#7553=DIRECTION('',(0.,0.540640817455599,-0.84125353283118));
#7554=DIRECTION('',(-1.,0.,0.));
#7555=DIRECTION('',(0.,0.540640817455599,-0.84125353283118));
#7556=DIRECTION('',(-1.,0.,0.));
#7557=DIRECTION('',(0.,0.540640817455599,-0.84125353283118));
#7558=DIRECTION('',(-1.,0.,0.));
#7559=DIRECTION('',(0.,0.,1.));
#7560=DIRECTION('',(-1.,0.,0.));
#7561=DIRECTION('',(0.,0.75574957435426,-0.654860733945284));
#7562=DIRECTION('',(-1.,0.,0.));
#7563=DIRECTION('',(0.,0.75574957435426,-0.654860733945284));
#7564=DIRECTION('',(-1.,0.,0.));
#7565=DIRECTION('',(0.,0.75574957435426,-0.654860733945284));
#7566=DIRECTION('',(-1.,0.,0.));
#7567=DIRECTION('',(0.,0.,1.));
#7568=DIRECTION('',(-1.,0.,0.));
#7569=DIRECTION('',(0.,0.90963199535452,-0.415415013001884));
#7570=DIRECTION('',(-1.,0.,0.));
#7571=DIRECTION('',(0.,0.90963199535452,-0.415415013001884));
#7572=DIRECTION('',(-1.,0.,0.));
#7573=DIRECTION('',(0.,0.90963199535452,-0.415415013001884));
#7574=DIRECTION('',(-1.,0.,0.));
#7575=DIRECTION('',(0.,0.,1.));
#7576=DIRECTION('',(-1.,0.,0.));
#7577=DIRECTION('',(0.,0.989821441880933,-0.142314838273282));
#7578=DIRECTION('',(-1.,0.,0.));
#7579=DIRECTION('',(0.,0.989821441880933,-0.142314838273282));
#7580=DIRECTION('',(-1.,0.,0.));
#7581=DIRECTION('',(0.,0.989821441880933,-0.142314838273282));
#7582=DIRECTION('',(-1.,0.,0.));
#7583=DIRECTION('',(0.,0.,1.));
#7584=DIRECTION('',(-1.,0.,0.));
#7585=DIRECTION('',(0.,0.,1.));
#7586=DIRECTION('',(-1.,0.,0.));
#7587=DIRECTION('',(-1.,0.,0.));
#7588=DIRECTION('',(-1.,0.,0.));
#7589=DIRECTION('',(0.,0.,1.));
#7590=DIRECTION('',(-1.,0.,0.));
#7591=DIRECTION('',(0.,0.,1.));
#7592=DIRECTION('',(-1.,0.,0.));
#7593=DIRECTION('',(-1.,0.,0.));
#7594=DIRECTION('',(0.,0.,1.));
#7595=DIRECTION('',(-1.,0.,0.));
#7596=DIRECTION('',(-1.,0.,0.));
#7597=DIRECTION('',(0.,0.,1.));
#7598=DIRECTION('',(-1.,0.,0.));
#7599=DIRECTION('',(-1.,0.,0.));
#7600=DIRECTION('',(-1.,0.,0.));
#7601=DIRECTION('',(0.,0.,1.));
#7602=DIRECTION('',(-1.,0.,0.));
#7603=DIRECTION('',(0.,0.,1.));
#7604=DIRECTION('',(-1.,0.,0.));
#7605=DIRECTION('',(-1.,0.,0.));
#7606=DIRECTION('',(-1.,0.,0.));
#7607=DIRECTION('',(0.,0.,1.));
#7608=DIRECTION('',(-1.,0.,0.));
#7609=DIRECTION('',(0.,0.,1.));
#7610=DIRECTION('',(-1.,0.,0.));
#7611=DIRECTION('',(-1.,0.,0.));
#7612=DIRECTION('',(-1.,0.,0.));
#7613=DIRECTION('',(0.,0.,1.));
#7614=DIRECTION('',(-1.,0.,0.));
#7615=DIRECTION('',(0.,0.,1.));
#7616=DIRECTION('',(-1.,0.,0.));
#7617=DIRECTION('',(-1.,0.,0.));
#7618=DIRECTION('',(0.,0.,1.));
#7619=DIRECTION('',(-1.,0.,0.));
#7620=DIRECTION('',(-1.,0.,0.));
#7621=DIRECTION('',(0.,0.,1.));
#7622=DIRECTION('',(-1.,0.,0.));
#7623=DIRECTION('',(-1.,0.,0.));
#7624=DIRECTION('',(-1.,0.,0.));
#7625=DIRECTION('',(0.,0.,1.));
#7626=DIRECTION('',(-1.,0.,0.));
#7627=DIRECTION('',(0.,0.,1.));
#7628=DIRECTION('',(-1.,0.,0.));
#7629=DIRECTION('',(-1.,0.,0.));
#7630=DIRECTION('',(0.,0.,1.));
#7631=DIRECTION('',(-1.,0.,0.));
#7632=DIRECTION('',(-1.,0.,0.));
#7633=DIRECTION('',(0.,0.,1.));
#7634=DIRECTION('',(-1.,0.,0.));
#7635=DIRECTION('',(-1.,0.,0.));
#7636=DIRECTION('',(-1.,0.,0.));
#7637=DIRECTION('',(0.,0.,1.));
#7638=DIRECTION('',(-1.,0.,0.));
#7639=DIRECTION('',(0.,0.,1.));
#7640=DIRECTION('',(-1.,0.,0.));
#7641=DIRECTION('',(-1.,0.,0.));
#7642=DIRECTION('',(-1.,0.,0.));
#7643=DIRECTION('',(0.,0.,1.));
#7644=DIRECTION('',(-1.,0.,0.));
#7645=DIRECTION('',(0.,0.,1.));
#7646=DIRECTION('',(-1.,0.,0.));
#7647=DIRECTION('',(-1.,0.,0.));
#7648=DIRECTION('',(0.,0.,1.));
#7649=DIRECTION('',(-1.,0.,0.));
#7650=DIRECTION('',(-1.,0.,0.));
#7651=DIRECTION('',(0.,0.,1.));
#7652=DIRECTION('',(-1.,0.,0.));
#7653=DIRECTION('',(-1.,0.,0.));
#7654=DIRECTION('',(-1.,0.,0.));
#7655=DIRECTION('',(0.,0.,1.));
#7656=DIRECTION('',(-1.,0.,0.));
#7657=DIRECTION('',(0.,0.,1.));
#7658=DIRECTION('',(-1.,0.,0.));
#7659=DIRECTION('',(-1.,0.,0.));
#7660=DIRECTION('',(0.,0.,1.));
#7661=DIRECTION('',(-1.,0.,0.));
#7662=DIRECTION('',(-1.,0.,0.));
#7663=DIRECTION('',(0.,0.,1.));
#7664=DIRECTION('',(-1.,0.,0.));
#7665=DIRECTION('',(-1.,0.,0.));
#7666=DIRECTION('',(0.,0.,1.));
#7667=DIRECTION('',(-1.,0.,0.));
#7668=DIRECTION('',(-1.,0.,0.));
#7669=DIRECTION('',(0.,0.,1.));
#7670=DIRECTION('',(-1.,0.,0.));
#7671=DIRECTION('',(-1.,0.,0.));
#7672=DIRECTION('',(0.,0.,1.));
#7673=DIRECTION('',(-1.,0.,0.));
#7674=DIRECTION('',(-1.,0.,0.));
#7675=DIRECTION('',(0.,0.,1.));
#7676=DIRECTION('',(-1.,0.,0.));
#7677=DIRECTION('',(-1.,0.,0.));
#7678=DIRECTION('',(-1.,0.,0.));
#7679=DIRECTION('',(0.,0.,1.));
#7680=DIRECTION('',(-1.,0.,0.));
#7681=DIRECTION('',(0.,0.,1.));
#7682=DIRECTION('',(-1.,0.,0.));
#7683=DIRECTION('',(-1.,0.,0.));
#7684=DIRECTION('',(-1.,0.,0.));
#7685=DIRECTION('',(0.,0.,1.));
#7686=DIRECTION('',(-1.,0.,0.));
#7687=DIRECTION('',(0.,0.,1.));
#7688=DIRECTION('',(-1.,0.,0.));
#7689=DIRECTION('',(-1.,0.,0.));
#7690=DIRECTION('',(0.,0.,1.));
#7691=DIRECTION('',(-1.,0.,0.));
#7692=DIRECTION('',(-1.,0.,0.));
#7693=DIRECTION('',(0.,0.,1.));
#7694=DIRECTION('',(-1.,0.,0.));
#7695=DIRECTION('',(-1.,0.,0.));
#7696=DIRECTION('',(0.,0.,1.));
#7697=DIRECTION('',(-1.,0.,0.));
#7698=DIRECTION('',(-1.,0.,0.));
#7699=DIRECTION('',(0.,0.,1.));
#7700=DIRECTION('',(-1.,0.,0.));
#7701=DIRECTION('',(-1.,0.,0.));
#7702=DIRECTION('',(0.,0.,1.));
#7703=DIRECTION('',(-1.,0.,0.));
#7704=DIRECTION('',(-1.,0.,0.));
#7705=DIRECTION('',(0.,0.,1.));
#7706=DIRECTION('',(-1.,0.,0.));
#7707=DIRECTION('',(-1.,0.,0.));
#7708=DIRECTION('',(-1.,0.,0.));
#7709=DIRECTION('',(0.,0.,1.));
#7710=DIRECTION('',(1.,0.,0.));
#7711=DIRECTION('',(0.,0.,-1.));
#7712=DIRECTION('',(-1.,0.,0.));
#7713=DIRECTION('',(0.,0.989821441880932,0.142314838273289));
#7714=DIRECTION('',(1.,0.,0.));
#7715=DIRECTION('',(0.,0.,-1.));
#7716=DIRECTION('',(-1.,0.,0.));
#7717=DIRECTION('',(0.,0.989821441880933,-0.142314838273282));
#7718=DIRECTION('',(-1.,0.,0.));
#7719=DIRECTION('',(0.,0.989821441880933,-0.142314838273282));
#7720=DIRECTION('',(1.,0.,0.));
#7721=DIRECTION('',(0.,0.,-1.));
#7722=DIRECTION('',(-1.,0.,0.));
#7723=DIRECTION('',(0.,0.90963199535452,-0.415415013001884));
#7724=DIRECTION('',(-1.,0.,0.));
#7725=DIRECTION('',(0.,0.90963199535452,-0.415415013001884));
#7726=DIRECTION('',(1.,0.,0.));
#7727=DIRECTION('',(0.,0.,-1.));
#7728=DIRECTION('',(-1.,0.,0.));
#7729=DIRECTION('',(0.,0.75574957435426,-0.654860733945284));
#7730=DIRECTION('',(-1.,0.,0.));
#7731=DIRECTION('',(0.,0.75574957435426,-0.654860733945284));
#7732=DIRECTION('',(1.,0.,0.));
#7733=DIRECTION('',(0.,0.,-1.));
#7734=DIRECTION('',(-1.,0.,0.));
#7735=DIRECTION('',(0.,0.540640817455599,-0.84125353283118));
#7736=DIRECTION('',(-1.,0.,0.));
#7737=DIRECTION('',(0.,0.540640817455599,-0.84125353283118));
#7738=DIRECTION('',(1.,0.,0.));
#7739=DIRECTION('',(0.,0.,-1.));
#7740=DIRECTION('',(-1.,0.,0.));
#7741=DIRECTION('',(0.,0.281732556841431,-0.959492973614497));
#7742=DIRECTION('',(-1.,0.,0.));
#7743=DIRECTION('',(0.,0.281732556841431,-0.959492973614497));
#7744=DIRECTION('',(-1.,0.,0.));
#7745=DIRECTION('',(0.,0.,1.));
#7746=DIRECTION('',(1.,0.,0.));
#7747=DIRECTION('',(0.,0.,-1.));
#7748=DIRECTION('',(-1.,0.,0.));
#7749=DIRECTION('',(0.,0.,-1.));
#7750=DIRECTION('',(-1.,0.,0.));
#7751=DIRECTION('',(0.,0.,-1.));
#7752=DIRECTION('',(1.,0.,0.));
#7753=DIRECTION('',(0.,0.,-1.));
#7754=DIRECTION('',(-1.,0.,0.));
#7755=DIRECTION('',(0.,-0.281732556841418,-0.959492973614501));
#7756=DIRECTION('',(-1.,0.,0.));
#7757=DIRECTION('',(0.,-0.281732556841418,-0.959492973614501));
#7758=DIRECTION('',(1.,0.,0.));
#7759=DIRECTION('',(0.,0.,-1.));
#7760=DIRECTION('',(-1.,0.,0.));
#7761=DIRECTION('',(0.,-0.540640817455587,-0.841253532831188));
#7762=DIRECTION('',(-1.,0.,0.));
#7763=DIRECTION('',(0.,-0.540640817455587,-0.841253532831188));
#7764=DIRECTION('',(1.,0.,0.));
#7765=DIRECTION('',(0.,0.,-1.));
#7766=DIRECTION('',(-1.,0.,0.));
#7767=DIRECTION('',(0.,-0.755749574354251,-0.654860733945294));
#7768=DIRECTION('',(-1.,0.,0.));
#7769=DIRECTION('',(0.,-0.755749574354251,-0.654860733945294));
#7770=DIRECTION('',(1.,0.,0.));
#7771=DIRECTION('',(0.,0.,-1.));
#7772=DIRECTION('',(-1.,0.,0.));
#7773=DIRECTION('',(0.,-0.909631995354514,-0.415415013001896));
#7774=DIRECTION('',(-1.,0.,0.));
#7775=DIRECTION('',(0.,-0.909631995354514,-0.415415013001896));
#7776=DIRECTION('',(1.,0.,0.));
#7777=DIRECTION('',(0.,0.,-1.));
#7778=DIRECTION('',(-1.,0.,0.));
#7779=DIRECTION('',(0.,-0.989821441880931,-0.142314838273295));
#7780=DIRECTION('',(-1.,0.,0.));
#7781=DIRECTION('',(0.,-0.989821441880931,-0.142314838273295));
#7782=DIRECTION('',(1.,0.,0.));
#7783=DIRECTION('',(0.,0.,-1.));
#7784=DIRECTION('',(-1.,0.,0.));
#7785=DIRECTION('',(0.,-0.989821441880934,0.142314838273276));
#7786=DIRECTION('',(-1.,0.,0.));
#7787=DIRECTION('',(0.,-0.989821441880934,0.142314838273276));
#7788=DIRECTION('',(1.,0.,0.));
#7789=DIRECTION('',(0.,0.,-1.));
#7790=DIRECTION('',(-1.,0.,0.));
#7791=DIRECTION('',(0.,-0.909631995354522,0.415415013001878));
#7792=DIRECTION('',(-1.,0.,0.));
#7793=DIRECTION('',(0.,-0.909631995354522,0.415415013001878));
#7794=DIRECTION('',(1.,0.,0.));
#7795=DIRECTION('',(0.,0.,-1.));
#7796=DIRECTION('',(-1.,0.,0.));
#7797=DIRECTION('',(0.,-0.755749574354264,0.654860733945279));
#7798=DIRECTION('',(-1.,0.,0.));
#7799=DIRECTION('',(0.,-0.755749574354264,0.654860733945279));
#7800=DIRECTION('',(1.,0.,0.));
#7801=DIRECTION('',(0.,0.,-1.));
#7802=DIRECTION('',(-1.,0.,0.));
#7803=DIRECTION('',(0.,-0.540640817455604,0.841253532831177));
#7804=DIRECTION('',(-1.,0.,0.));
#7805=DIRECTION('',(0.,-0.540640817455604,0.841253532831177));
#7806=DIRECTION('',(1.,0.,0.));
#7807=DIRECTION('',(0.,0.,-1.));
#7808=DIRECTION('',(-1.,0.,0.));
#7809=DIRECTION('',(0.,-0.281732556841436,0.959492973614495));
#7810=DIRECTION('',(-1.,0.,0.));
#7811=DIRECTION('',(0.,-0.281732556841436,0.959492973614495));
#7812=DIRECTION('',(1.,0.,0.));
#7813=DIRECTION('',(0.,0.,-1.));
#7814=DIRECTION('',(-1.,0.,0.));
#7815=DIRECTION('',(0.,-6.53887346783621E-15,1.));
#7816=DIRECTION('',(-1.,0.,0.));
#7817=DIRECTION('',(0.,-6.53887346783621E-15,1.));
#7818=DIRECTION('',(1.,0.,0.));
#7819=DIRECTION('',(0.,0.,-1.));
#7820=DIRECTION('',(-1.,0.,0.));
#7821=DIRECTION('',(0.,0.281732556841424,0.959492973614499));
#7822=DIRECTION('',(-1.,0.,0.));
#7823=DIRECTION('',(0.,0.281732556841424,0.959492973614499));
#7824=DIRECTION('',(1.,0.,0.));
#7825=DIRECTION('',(0.,0.,-1.));
#7826=DIRECTION('',(-1.,0.,0.));
#7827=DIRECTION('',(0.,0.540640817455593,0.841253532831184));
#7828=DIRECTION('',(-1.,0.,0.));
#7829=DIRECTION('',(0.,0.540640817455593,0.841253532831184));
#7830=DIRECTION('',(1.,0.,0.));
#7831=DIRECTION('',(0.,0.,-1.));
#7832=DIRECTION('',(-1.,0.,0.));
#7833=DIRECTION('',(0.,0.755749574354255,0.654860733945289));
#7834=DIRECTION('',(-1.,0.,0.));
#7835=DIRECTION('',(0.,0.755749574354255,0.654860733945289));
#7836=DIRECTION('',(1.,0.,0.));
#7837=DIRECTION('',(0.,0.,-1.));
#7838=DIRECTION('',(-1.,0.,0.));
#7839=DIRECTION('',(0.,0.909631995354517,0.41541501300189));
#7840=DIRECTION('',(-1.,0.,0.));
#7841=DIRECTION('',(0.,0.909631995354517,0.41541501300189));
#7842=DIRECTION('',(1.,0.,0.));
#7843=DIRECTION('',(0.,0.,-1.));
#7844=DIRECTION('',(-1.,0.,0.));
#7845=DIRECTION('',(0.,0.989821441880932,0.142314838273289));
#7846=DIRECTION('',(-1.,0.,0.));
#7847=DIRECTION('',(0.,0.,1.));
#7848=DIRECTION('',(-1.,0.,0.));
#7849=DIRECTION('',(-1.,0.,0.));
#7850=DIRECTION('',(-1.,0.,0.));
#7851=DIRECTION('',(0.,0.,1.));
#7852=DIRECTION('',(-1.,0.,0.));
#7853=DIRECTION('',(-1.,0.,0.));
#7854=DIRECTION('',(0.,0.,1.));
#7855=DIRECTION('',(-1.,0.,0.));
#7856=DIRECTION('',(-1.,0.,0.));
#7857=DIRECTION('',(0.,0.,1.));
#7858=DIRECTION('',(-1.,0.,0.));
#7859=DIRECTION('',(0.,0.,1.));
#7860=DIRECTION('',(-1.,0.,0.));
#7861=DIRECTION('',(-1.,0.,0.));
#7862=DIRECTION('',(0.,0.,1.));
#7863=DIRECTION('',(-1.,0.,0.));
#7864=DIRECTION('',(-1.,0.,0.));
#7865=DIRECTION('',(0.,0.,1.));
#7866=DIRECTION('',(-1.,0.,0.));
#7867=DIRECTION('',(0.,0.,1.));
#7868=DIRECTION('',(-1.,0.,0.));
#7869=DIRECTION('',(-1.,0.,0.));
#7870=DIRECTION('',(0.,0.,1.));
#7871=DIRECTION('',(-1.,0.,0.));
#7872=DIRECTION('',(-1.,0.,0.));
#7873=DIRECTION('',(0.,0.,1.));
#7874=DIRECTION('',(-1.,0.,0.));
#7875=DIRECTION('',(0.,0.,1.));
#7876=DIRECTION('',(-1.,0.,0.));
#7877=DIRECTION('',(-1.,0.,0.));
#7878=DIRECTION('',(0.,0.,1.));
#7879=DIRECTION('',(-1.,0.,0.));
#7880=DIRECTION('',(-1.,0.,0.));
#7881=DIRECTION('',(0.,0.,1.));
#7882=DIRECTION('',(-1.,0.,0.));
#7883=DIRECTION('',(0.,0.,1.));
#7884=DIRECTION('',(-1.,0.,0.));
#7885=DIRECTION('',(-1.,0.,0.));
#7886=DIRECTION('',(0.,0.,1.));
#7887=DIRECTION('',(-1.,0.,0.));
#7888=DIRECTION('',(-1.,0.,0.));
#7889=DIRECTION('',(0.,0.,1.));
#7890=DIRECTION('',(-1.,0.,0.));
#7891=DIRECTION('',(0.,0.,1.));
#7892=DIRECTION('',(-1.,0.,0.));
#7893=DIRECTION('',(-1.,0.,0.));
#7894=DIRECTION('',(0.,0.,1.));
#7895=DIRECTION('',(-1.,0.,0.));
#7896=DIRECTION('',(-1.,0.,0.));
#7897=DIRECTION('',(0.,0.,1.));
#7898=DIRECTION('',(-1.,0.,0.));
#7899=DIRECTION('',(0.,0.,1.));
#7900=DIRECTION('',(-1.,0.,0.));
#7901=DIRECTION('',(-1.,0.,0.));
#7902=DIRECTION('',(0.,0.,1.));
#7903=DIRECTION('',(-1.,0.,0.));
#7904=DIRECTION('',(-1.,0.,0.));
#7905=DIRECTION('',(0.,0.,1.));
#7906=DIRECTION('',(-1.,0.,0.));
#7907=DIRECTION('',(0.,0.,1.));
#7908=DIRECTION('',(-1.,0.,0.));
#7909=DIRECTION('',(-1.,0.,0.));
#7910=DIRECTION('',(0.,0.,1.));
#7911=DIRECTION('',(-1.,0.,0.));
#7912=DIRECTION('',(-1.,0.,0.));
#7913=DIRECTION('',(0.,0.,1.));
#7914=DIRECTION('',(-1.,0.,0.));
#7915=DIRECTION('',(0.,0.,1.));
#7916=DIRECTION('',(-1.,0.,0.));
#7917=DIRECTION('',(-1.,0.,0.));
#7918=DIRECTION('',(0.,0.,1.));
#7919=DIRECTION('',(-1.,0.,0.));
#7920=DIRECTION('',(-1.,0.,0.));
#7921=DIRECTION('',(0.,0.,1.));
#7922=DIRECTION('',(-1.,0.,0.));
#7923=DIRECTION('',(0.,0.,1.));
#7924=DIRECTION('',(-1.,0.,0.));
#7925=DIRECTION('',(-1.,0.,0.));
#7926=DIRECTION('',(0.,0.,1.));
#7927=DIRECTION('',(-1.,0.,0.));
#7928=DIRECTION('',(-1.,0.,0.));
#7929=DIRECTION('',(0.,0.,1.));
#7930=DIRECTION('',(-1.,0.,0.));
#7931=DIRECTION('',(0.,0.,1.));
#7932=DIRECTION('',(-1.,0.,0.));
#7933=DIRECTION('',(-1.,0.,0.));
#7934=DIRECTION('',(0.,0.,1.));
#7935=DIRECTION('',(-1.,0.,0.));
#7936=DIRECTION('',(-1.,0.,0.));
#7937=DIRECTION('',(0.,0.,1.));
#7938=DIRECTION('',(-1.,0.,0.));
#7939=DIRECTION('',(0.,0.,1.));
#7940=DIRECTION('',(-1.,0.,0.));
#7941=DIRECTION('',(-1.,0.,0.));
#7942=DIRECTION('',(0.,0.,1.));
#7943=DIRECTION('',(-1.,0.,0.));
#7944=DIRECTION('',(-1.,0.,0.));
#7945=DIRECTION('',(0.,0.,1.));
#7946=DIRECTION('',(-1.,0.,0.));
#7947=DIRECTION('',(0.,0.,1.));
#7948=DIRECTION('',(-1.,0.,0.));
#7949=DIRECTION('',(-1.,0.,0.));
#7950=DIRECTION('',(0.,0.,1.));
#7951=DIRECTION('',(-1.,0.,0.));
#7952=DIRECTION('',(-1.,0.,0.));
#7953=DIRECTION('',(0.,0.,1.));
#7954=DIRECTION('',(-1.,0.,0.));
#7955=DIRECTION('',(0.,0.,1.));
#7956=DIRECTION('',(-1.,0.,0.));
#7957=DIRECTION('',(-1.,0.,0.));
#7958=DIRECTION('',(0.,0.,1.));
#7959=DIRECTION('',(-1.,0.,0.));
#7960=DIRECTION('',(-1.,0.,0.));
#7961=DIRECTION('',(0.,0.,1.));
#7962=DIRECTION('',(-1.,0.,0.));
#7963=DIRECTION('',(0.,0.,1.));
#7964=DIRECTION('',(-1.,0.,0.));
#7965=DIRECTION('',(-1.,0.,0.));
#7966=DIRECTION('',(0.,0.,1.));
#7967=DIRECTION('',(-1.,0.,0.));
#7968=DIRECTION('',(-1.,0.,0.));
#7969=DIRECTION('',(0.,0.,1.));
#7970=DIRECTION('',(-1.,0.,0.));
#7971=DIRECTION('',(0.,0.,1.));
#7972=DIRECTION('',(-1.,0.,0.));
#7973=DIRECTION('',(-1.,0.,0.));
#7974=DIRECTION('',(0.,0.,1.));
#7975=DIRECTION('',(-1.,0.,0.));
#7976=DIRECTION('',(-1.,0.,0.));
#7977=DIRECTION('',(0.,0.,1.));
#7978=DIRECTION('',(-1.,0.,0.));
#7979=DIRECTION('',(0.,0.,1.));
#7980=DIRECTION('',(-1.,0.,0.));
#7981=DIRECTION('',(-1.,0.,0.));
#7982=DIRECTION('',(0.,0.,1.));
#7983=DIRECTION('',(-1.,0.,0.));
#7984=DIRECTION('',(-1.,0.,0.));
#7985=DIRECTION('',(0.,0.,1.));
#7986=DIRECTION('',(-1.,0.,0.));
#7987=DIRECTION('',(0.,0.,1.));
#7988=DIRECTION('',(-1.,0.,0.));
#7989=DIRECTION('',(-1.,0.,0.));
#7990=DIRECTION('',(0.,0.,1.));
#7991=DIRECTION('',(-1.,0.,0.));
#7992=DIRECTION('',(-1.,0.,0.));
#7993=DIRECTION('',(0.,0.,1.));
#7994=DIRECTION('',(-1.,0.,0.));
#7995=DIRECTION('',(0.,0.,1.));
#7996=DIRECTION('',(-1.,0.,0.));
#7997=DIRECTION('',(-1.,0.,0.));
#7998=DIRECTION('',(0.,0.,1.));
#7999=DIRECTION('',(-1.,0.,0.));
#8000=DIRECTION('',(-1.,0.,0.));
#8001=DIRECTION('',(0.,0.,1.));
#8002=DIRECTION('',(-1.,0.,0.));
#8003=DIRECTION('',(0.,0.,1.));
#8004=DIRECTION('',(-1.,0.,0.));
#8005=DIRECTION('',(-1.,0.,0.));
#8006=DIRECTION('',(0.,0.,1.));
#8007=DIRECTION('',(-1.,0.,0.));
#8008=DIRECTION('',(-1.,0.,0.));
#8009=DIRECTION('',(0.,0.,1.));
#8010=DIRECTION('',(-1.,0.,0.));
#8011=DIRECTION('',(0.,0.,1.));
#8012=DIRECTION('',(-1.,0.,0.));
#8013=DIRECTION('',(-1.,0.,0.));
#8014=DIRECTION('',(0.,0.,1.));
#8015=DIRECTION('',(-1.,0.,0.));
#8016=DIRECTION('',(-1.,0.,0.));
#8017=DIRECTION('',(0.,0.,1.));
#8018=DIRECTION('',(-1.,0.,0.));
#8019=DIRECTION('',(0.,0.,1.));
#8020=DIRECTION('',(-1.,0.,0.));
#8021=DIRECTION('',(-1.,0.,0.));
#8022=DIRECTION('',(0.,0.,1.));
#8023=DIRECTION('',(-1.,0.,0.));
#8024=DIRECTION('',(-1.,0.,0.));
#8025=DIRECTION('',(0.,0.,1.));
#8026=DIRECTION('',(1.,0.,0.));
#8027=DIRECTION('',(0.,0.,-1.));
#8028=DIRECTION('',(1.,0.,0.));
#8029=DIRECTION('',(0.,0.,-1.));
#8030=DIRECTION('',(1.,0.,0.));
#8031=DIRECTION('',(0.,0.,-1.));
#8032=DIRECTION('',(1.,0.,0.));
#8033=DIRECTION('',(0.,0.,-1.));
#8034=DIRECTION('',(1.,0.,0.));
#8035=DIRECTION('',(0.,0.,-1.));
#8036=DIRECTION('',(1.,0.,0.));
#8037=DIRECTION('',(0.,0.,-1.));
#8038=DIRECTION('',(1.,0.,0.));
#8039=DIRECTION('',(0.,0.,-1.));
#8040=DIRECTION('',(-1.,0.,0.));
#8041=DIRECTION('',(0.,0.,1.));
#8042=DIRECTION('',(1.,0.,0.));
#8043=DIRECTION('',(0.,0.,-1.));
#8044=DIRECTION('',(1.,0.,0.));
#8045=DIRECTION('',(0.,0.,-1.));
#8046=DIRECTION('',(1.,0.,0.));
#8047=DIRECTION('',(0.,0.,-1.));
#8048=DIRECTION('',(1.,0.,0.));
#8049=DIRECTION('',(0.,0.,-1.));
#8050=DIRECTION('',(-1.,0.,0.));
#8051=DIRECTION('',(0.,0.,1.));
#8052=DIRECTION('',(1.,0.,0.));
#8053=DIRECTION('',(0.,0.,-1.));
#8054=DIRECTION('',(0.362554980561836,-0.931962384471501,-1.98669103517402E-16));
#8055=DIRECTION('',(4.20741553168918E-17,-1.96805055665783E-16,1.));
#8056=DIRECTION('',(1.,0.,0.));
#8057=DIRECTION('',(0.,0.,-1.));
#8058=DIRECTION('',(1.,0.,0.));
#8059=DIRECTION('',(0.,0.,-1.));
#8060=DIRECTION('',(1.,0.,0.));
#8061=DIRECTION('',(1.,0.,0.));
#8062=DIRECTION('',(0.,0.,-1.));
#8063=DIRECTION('',(1.,0.,0.));
#8064=DIRECTION('',(1.,0.,0.));
#8065=DIRECTION('',(0.,0.,-1.));
#8066=DIRECTION('',(1.,0.,0.));
#8067=DIRECTION('',(0.,0.,-1.));
#8068=DIRECTION('',(1.,0.,0.));
#8069=DIRECTION('',(1.,0.,0.));
#8070=DIRECTION('',(0.,0.,-1.));
#8071=DIRECTION('',(1.,0.,0.));
#8072=DIRECTION('',(0.,0.,-1.));
#8073=DIRECTION('',(-1.,0.,0.));
#8074=DIRECTION('',(0.,0.,-1.));
#8075=DIRECTION('',(1.,0.,0.));
#8076=DIRECTION('',(-1.,0.,0.));
#8077=DIRECTION('',(0.,0.,-1.));
#8078=DIRECTION('',(0.,1.,0.));
#8079=DIRECTION('',(0.,0.,1.));
#8080=DIRECTION('',(0.,0.,1.));
#8081=DIRECTION('',(0.,0.,1.));
#8082=DIRECTION('',(1.,0.,0.));
#8083=DIRECTION('',(0.,0.,-1.));
#8084=DIRECTION('',(1.,0.,0.));
#8085=DIRECTION('',(0.,0.,-1.));
#8086=DIRECTION('',(1.,0.,0.));
#8087=DIRECTION('',(0.,0.,-1.));
#8088=DIRECTION('',(1.,0.,0.));
#8089=DIRECTION('',(0.,0.,-1.));
#8090=DIRECTION('',(1.,0.,0.));
#8091=DIRECTION('',(0.,0.,-1.));
#8092=DIRECTION('',(0.979019048375703,0.203768748628273,5.30625654556973E-18));
#8093=DIRECTION('',(-5.5706883703669E-17,2.93687610195238E-16,-1.));
#8094=DIRECTION('',(-1.,0.,0.));
#8095=DIRECTION('',(0.,0.,1.));
#8096=DIRECTION('',(0.,1.27620930369834E-17,1.));
#8097=DIRECTION('',(0.,-1.,1.27620930369834E-17));
#8098=DIRECTION('',(-1.,0.,0.));
#8099=DIRECTION('',(0.,0.,1.));
#8100=DIRECTION('',(-1.,0.,0.));
#8101=DIRECTION('',(0.,0.,1.));
#8102=DIRECTION('',(-1.,0.,0.));
#8103=DIRECTION('',(0.,0.,1.));
#8104=DIRECTION('',(-1.,0.,0.));
#8105=DIRECTION('',(-1.,0.,0.));
#8106=DIRECTION('',(0.,0.,1.));
#8107=DIRECTION('',(-1.,0.,0.));
#8108=DIRECTION('',(-1.,0.,0.));
#8109=DIRECTION('',(0.,0.,1.));
#8110=DIRECTION('',(0.,1.27620930369834E-17,1.));
#8111=DIRECTION('',(0.,-1.,1.27620930369834E-17));
#8112=DIRECTION('',(-1.,0.,0.));
#8113=DIRECTION('',(0.,0.,1.));
#8114=DIRECTION('',(-1.,0.,0.));
#8115=DIRECTION('',(0.,0.,1.));
#8116=DIRECTION('',(-1.,0.,0.));
#8117=DIRECTION('',(-1.,0.,0.));
#8118=DIRECTION('',(0.,1.,-1.12666127576541E-17));
#8119=DIRECTION('',(0.,1.12666127576541E-17,1.));
#8120=DIRECTION('',(-1.,0.,0.));
#8121=DIRECTION('',(-1.,0.,0.));
#8122=DIRECTION('',(0.,1.27620930369834E-17,1.));
#8123=DIRECTION('',(0.,-1.,1.27620930369834E-17));
#8124=DIRECTION('',(0.,1.27620930369834E-17,1.));
#8125=DIRECTION('',(0.,-1.,1.27620930369834E-17));
#8126=DIRECTION('',(-1.,0.,0.));
#8127=DIRECTION('',(0.,1.27620930369834E-17,1.));
#8128=DIRECTION('',(0.,-1.,1.27620930369834E-17));
#8129=DIRECTION('',(-1.,0.,0.));
#8130=DIRECTION('',(-1.,0.,0.));
#8131=DIRECTION('',(0.,0.,1.));
#8132=DIRECTION('',(-1.,0.,0.));
#8133=DIRECTION('',(0.,0.,1.));
#8134=DIRECTION('',(-1.,0.,0.));
#8135=DIRECTION('',(0.,0.,1.));
#8136=DIRECTION('',(-1.,0.,0.));
#8137=DIRECTION('',(0.,0.,1.));
#8138=DIRECTION('',(-1.,0.,0.));
#8139=DIRECTION('',(0.,0.,1.));
#8140=DIRECTION('',(-1.,0.,0.));
#8141=DIRECTION('',(0.,0.,1.));
#8142=DIRECTION('',(-1.,0.,0.));
#8143=DIRECTION('',(0.,0.,1.));
#8144=DIRECTION('',(-1.,0.,0.));
#8145=DIRECTION('',(0.,0.,1.));
#8146=DIRECTION('',(-0.187508504269887,0.982262979464497,7.16278451644582E-17));
#8147=DIRECTION('',(6.12323399573677E-17,-6.12323399573677E-17,1.));
#8148=DIRECTION('',(0.,0.,1.));
#8149=DIRECTION('',(1.,0.,0.));
#8150=DIRECTION('',(0.,1.,0.));
#8151=DIRECTION('',(0.,0.,1.));
#8152=DIRECTION('',(0.,1.,0.));
#8153=DIRECTION('',(0.,0.,1.));
#8154=DIRECTION('',(0.,1.,0.));
#8155=DIRECTION('',(0.,0.,1.));
#8156=DIRECTION('',(1.,0.,0.));
#8157=DIRECTION('',(0.,1.,0.));
#8158=DIRECTION('',(0.,0.,1.));
#8159=DIRECTION('',(-1.,0.,0.));
#8160=DIRECTION('',(0.,1.,0.));
#8161=DIRECTION('',(0.,0.,1.));
#8162=DIRECTION('',(0.,1.,0.));
#8163=DIRECTION('',(0.,0.,1.));
#8164=DIRECTION('',(0.,1.,0.));
#8165=DIRECTION('',(0.,0.,1.));
#8166=DIRECTION('',(-1.,0.,0.));
#8167=DIRECTION('',(0.,1.,0.));
#8168=DIRECTION('',(0.,0.,1.));
#8169=DIRECTION('',(1.,0.,0.));
#8170=DIRECTION('',(0.,1.,0.));
#8171=DIRECTION('',(0.,0.,1.));
#8172=DIRECTION('',(0.,1.,0.));
#8173=DIRECTION('',(0.,0.,1.));
#8174=DIRECTION('',(0.,-1.,0.));
#8175=DIRECTION('',(0.,0.,-1.));
#8176=DIRECTION('',(0.,-1.,0.));
#8177=DIRECTION('',(0.,-1.,0.));
#8178=DIRECTION('',(0.,0.,-1.));
#8179=DIRECTION('',(-1.,0.,0.));
#8180=DIRECTION('',(0.,-1.,0.));
#8181=DIRECTION('',(0.,-1.,0.));
#8182=DIRECTION('',(0.,0.,-1.));
#8183=DIRECTION('',(0.,-1.,0.));
#8184=DIRECTION('',(0.,0.,1.));
#8185=DIRECTION('',(1.,0.,0.));
#8186=DIRECTION('',(0.,-1.,0.));
#8187=DIRECTION('',(0.,0.,-1.));
#8188=DIRECTION('',(0.,-1.,0.));
#8189=DIRECTION('',(0.,0.,-1.));
#8190=DIRECTION('',(0.806697943703821,0.59096398166388,-1.32098952905852E-17));
#8191=DIRECTION('',(-0.59096398166388,0.806697943703821,8.55851492407836E-17));
#8192=DIRECTION('',(0.,1.,0.));
#8193=DIRECTION('',(0.,0.,1.));
#8194=DIRECTION('',(0.,1.,0.));
#8195=DIRECTION('',(0.,0.,1.));
#8196=DIRECTION('',(0.,1.,0.));
#8197=DIRECTION('',(0.,0.,1.));
#8198=DIRECTION('',(0.,1.,0.));
#8199=DIRECTION('',(0.,0.,1.));
#8200=DIRECTION('',(0.,1.,0.));
#8201=DIRECTION('',(0.,0.,1.));
#8202=DIRECTION('',(0.,1.,0.));
#8203=DIRECTION('',(0.,0.,1.));
#8204=DIRECTION('',(0.,1.,0.));
#8205=DIRECTION('',(0.,0.,1.));
#8206=DIRECTION('',(0.,1.,0.));
#8207=DIRECTION('',(0.,0.,1.));
#8208=DIRECTION('',(0.,1.,0.));
#8209=DIRECTION('',(0.,0.,1.));
#8210=DIRECTION('',(0.,-1.,0.));
#8211=DIRECTION('',(0.,0.,-1.));
#8212=DIRECTION('',(0.,1.,0.));
#8213=DIRECTION('',(0.,0.,1.));
#8214=DIRECTION('',(0.,1.,0.));
#8215=DIRECTION('',(0.,0.,1.));
#8216=DIRECTION('',(0.,1.,0.));
#8217=DIRECTION('',(0.,0.,1.));
#8218=DIRECTION('',(0.,-1.,0.));
#8219=DIRECTION('',(0.,0.,-1.));
#8220=DIRECTION('',(0.,1.,0.));
#8221=DIRECTION('',(0.,0.,1.));
#8222=DIRECTION('',(0.,1.,0.));
#8223=DIRECTION('',(0.,0.,1.));
#8224=DIRECTION('',(0.,1.,0.));
#8225=DIRECTION('',(0.,0.,1.));
#8226=DIRECTION('',(0.,1.,0.));
#8227=DIRECTION('',(0.,0.,1.));
#8228=DIRECTION('',(0.,1.,0.));
#8229=DIRECTION('',(0.,0.,1.));
#8230=DIRECTION('',(0.,1.,0.));
#8231=DIRECTION('',(0.,0.,1.));
#8232=DIRECTION('',(0.,-1.,0.));
#8233=DIRECTION('',(0.,0.,-1.));
#8234=DIRECTION('',(0.,1.,0.));
#8235=DIRECTION('',(0.,0.,1.));
#8236=DIRECTION('',(0.,1.,0.));
#8237=DIRECTION('',(0.,0.,1.));
#8238=DIRECTION('',(0.,-1.,0.));
#8239=DIRECTION('',(0.,0.,-1.));
#8240=DIRECTION('',(0.,1.,0.));
#8241=DIRECTION('',(0.,0.,1.));
#8242=DIRECTION('',(0.,1.,0.));
#8243=DIRECTION('',(0.,0.,1.));
#8244=DIRECTION('',(0.,-1.,0.));
#8245=DIRECTION('',(0.,0.,-1.));
#8246=DIRECTION('',(0.,1.,0.));
#8247=DIRECTION('',(0.,0.,1.));
#8248=DIRECTION('',(0.,-1.,0.));
#8249=DIRECTION('',(0.,0.,-1.));
#8250=DIRECTION('',(0.,-1.,0.));
#8251=DIRECTION('',(0.,0.,-1.));
#8252=DIRECTION('',(0.,1.,0.));
#8253=DIRECTION('',(0.,0.,1.));
#8254=DIRECTION('',(0.,-1.,0.));
#8255=DIRECTION('',(0.,0.,-1.));
#8256=DIRECTION('',(-6.12323399573677E-17,-1.,-6.12323399573677E-17));
#8257=DIRECTION('',(1.,-6.12323399573677E-17,-6.12323399573677E-17));
#8258=DIRECTION('',(0.,1.,0.));
#8259=DIRECTION('',(0.,0.,1.));
#8260=DIRECTION('',(0.,1.,0.));
#8261=DIRECTION('',(0.,0.,1.));
#8262=DIRECTION('',(0.,-1.,0.));
#8263=DIRECTION('',(0.,0.,1.));
#8264=DIRECTION('',(-0.034645075969331,0.,-0.999399679162986));
#8265=DIRECTION('',(0.,1.,0.));
#8266=DIRECTION('',(0.,0.,1.));
#8267=DIRECTION('',(-0.0346450759693315,0.,-0.999399679162986));
#8268=DIRECTION('',(-0.0346450759693315,0.,0.999399679162986));
#8269=DIRECTION('',(0.,1.,0.));
#8270=DIRECTION('',(0.,0.,1.));
#8271=DIRECTION('',(-0.034645075969331,0.,0.999399679162986));
#8272=DIRECTION('',(0.,-1.,0.));
#8273=DIRECTION('',(0.,0.,-1.));
#8274=DIRECTION('',(0.,1.,0.));
#8275=DIRECTION('',(0.,0.,-1.));
#8276=DIRECTION('',(1.,0.,0.));
#8277=DIRECTION('',(0.,1.,0.));
#8278=DIRECTION('',(0.,0.,1.));
#8279=DIRECTION('',(0.,1.,0.));
#8280=DIRECTION('',(0.,0.,1.));
#8281=DIRECTION('',(0.,1.,0.));
#8282=DIRECTION('',(0.,0.,1.));
#8283=DIRECTION('',(1.,0.,0.));
#8284=DIRECTION('',(0.,1.,0.));
#8285=DIRECTION('',(0.,0.,-1.));
#8286=DIRECTION('',(0.,-1.,0.));
#8287=DIRECTION('',(0.,0.,-1.));
#8288=DIRECTION('',(-0.034645075969331,0.,0.999399679162986));
#8289=DIRECTION('',(0.,1.,0.));
#8290=DIRECTION('',(0.,0.,1.));
#8291=DIRECTION('',(-0.0346450759693315,0.,0.999399679162986));
#8292=DIRECTION('',(-0.0346450759693315,0.,-0.999399679162986));
#8293=DIRECTION('',(0.,1.,0.));
#8294=DIRECTION('',(0.,0.,1.));
#8295=DIRECTION('',(-0.034645075969331,0.,-0.999399679162986));
#8296=DIRECTION('',(0.,-1.,0.));
#8297=DIRECTION('',(0.,0.,1.));
#8298=DIRECTION('',(0.,1.,0.));
#8299=DIRECTION('',(0.,0.,1.));
#8300=DIRECTION('',(0.,-1.,0.));
#8301=DIRECTION('',(0.,0.,-1.));
#8302=DIRECTION('',(0.,-1.,0.));
#8303=DIRECTION('',(0.,-1.,0.));
#8304=DIRECTION('',(0.,-1.,0.));
#8305=DIRECTION('',(0.,0.,-1.));
#8306=DIRECTION('',(0.,-1.,0.));
#8307=DIRECTION('',(-0.999399679162986,0.,0.034645075969331));
#8308=DIRECTION('',(0.034645075969331,0.,0.999399679162986));
#8309=DIRECTION('',(0.,-1.,0.));
#8310=DIRECTION('',(0.,-1.,0.));
#8311=DIRECTION('',(0.,0.,-1.));
#8312=DIRECTION('',(0.,-1.,0.));
#8313=DIRECTION('',(-0.999399679162986,0.,0.0346450759693315));
#8314=DIRECTION('',(0.0346450759693315,0.,0.999399679162986));
#8315=DIRECTION('',(0.,-1.,0.));
#8316=DIRECTION('',(0.999399679162986,0.,0.0346450759693315));
#8317=DIRECTION('',(0.0346450759693315,0.,-0.999399679162986));
#8318=DIRECTION('',(0.,-1.,0.));
#8319=DIRECTION('',(0.,-1.,0.));
#8320=DIRECTION('',(0.,0.,-1.));
#8321=DIRECTION('',(0.,-1.,0.));
#8322=DIRECTION('',(0.999399679162986,0.,0.034645075969331));
#8323=DIRECTION('',(0.034645075969331,0.,-0.999399679162986));
#8324=DIRECTION('',(0.,-1.,0.));
#8325=DIRECTION('',(0.,-1.,0.));
#8326=DIRECTION('',(0.,0.,-1.));
#8327=DIRECTION('',(0.,-1.,0.));
#8328=DIRECTION('',(0.,-1.,0.));
#8329=DIRECTION('',(0.,0.,-1.));
#8330=DIRECTION('',(0.,-1.,0.));
#8331=DIRECTION('',(0.,0.,-1.));
#8332=DIRECTION('',(-1.,0.,0.));
#8333=DIRECTION('',(0.,-1.,0.));
#8334=DIRECTION('',(0.,0.,-1.));
#8335=DIRECTION('',(-0.124247662884138,-0.992251237473569,-1.90052444559479E-16));
#8336=DIRECTION('',(0.992251237473569,-0.124247662884138,-6.62007008890972E-17));
#8337=DIRECTION('',(0.,0.,-1.));
#8338=DIRECTION('',(-1.,0.,0.));
#8339=DIRECTION('',(1.,0.,0.));
#8340=DIRECTION('',(0.,0.,-1.));
#8341=DIRECTION('',(-1.,0.,0.));
#8342=DIRECTION('',(0.,0.,-1.));
#8343=DIRECTION('',(-1.,0.,0.));
#8344=DIRECTION('',(0.,0.,1.));
#8345=DIRECTION('',(1.,0.,0.));
#8346=DIRECTION('',(0.,0.,-1.));
#8347=DIRECTION('',(-1.,0.,0.));
#8348=DIRECTION('',(0.,0.,-1.));
#8349=DIRECTION('',(-1.,0.,0.));
#8350=DIRECTION('',(0.,0.,1.));
#8351=DIRECTION('',(1.,0.,0.));
#8352=DIRECTION('',(0.,0.,-1.));
#8353=DIRECTION('',(-1.,0.,0.));
#8354=DIRECTION('',(0.,0.,1.));
#8355=DIRECTION('',(1.,0.,0.));
#8356=DIRECTION('',(0.,0.,1.));
#8357=DIRECTION('',(1.,0.,0.));
#8358=DIRECTION('',(0.,0.,-1.));
#8359=DIRECTION('',(-1.,0.,0.));
#8360=DIRECTION('',(1.,0.,0.));
#8361=DIRECTION('',(0.,0.,-1.));
#8362=DIRECTION('',(-1.,0.,0.));
#8363=DIRECTION('',(0.,0.,1.));
#8364=DIRECTION('',(1.,0.,0.));
#8365=DIRECTION('',(0.,0.,1.));
#8366=DIRECTION('',(1.,0.,0.));
#8367=DIRECTION('',(0.,0.,1.));
#8368=DIRECTION('',(1.,0.,0.));
#8369=DIRECTION('',(0.,0.,-1.));
#8370=DIRECTION('',(-1.,0.,0.));
#8371=DIRECTION('',(0.,0.,1.));
#8372=DIRECTION('',(1.,0.,0.));
#8373=DIRECTION('',(0.,0.,-1.));
#8374=DIRECTION('',(-1.,0.,0.));
#8375=DIRECTION('',(0.,0.,-1.));
#8376=DIRECTION('',(-1.,0.,0.));
#8377=DIRECTION('',(0.,0.,-1.));
#8378=DIRECTION('',(-1.,0.,0.));
#8379=DIRECTION('',(0.,0.,1.));
#8380=DIRECTION('',(1.,0.,0.));
#8381=DIRECTION('',(1.,0.,0.));
#8382=DIRECTION('',(1.,0.,0.));
#8383=DIRECTION('',(0.,-1.,0.));
#8384=DIRECTION('',(0.,0.,-1.));
#8385=DIRECTION('',(0.,-1.,0.));
#8386=DIRECTION('',(0.,0.,-1.));
#8387=DIRECTION('',(0.,0.,1.));
#8388=DIRECTION('',(1.,0.,0.));
#8389=DIRECTION('',(4.15538270412058E-17,-1.9546753058265E-16,1.));
#8390=DIRECTION('',(-0.931962384471501,-0.362554980561836,-3.21411230176243E-17));
#8391=CARTESIAN_POINT('',(0.,0.,0.));
#8392=CARTESIAN_POINT('',(0.,0.03,0.));
#8393=CARTESIAN_POINT('',(0.,0.001,0.));
#8394=CARTESIAN_POINT('',(0.,0.001,-0.06));
#8395=CARTESIAN_POINT('',(0.,0.03,0.));
#8396=CARTESIAN_POINT('',(0.,0.03,0.06));
#8397=CARTESIAN_POINT('',(-0.0039149404887588,0.0139224634434835,0.0598960985083079));
#8398=CARTESIAN_POINT('',(-0.00554222253988876,0.00999901026546572,0.0597389564762431));
#8399=CARTESIAN_POINT('',(-0.00391616935168617,0.00608149549465367,0.0598958978797615));
#8400=CARTESIAN_POINT('',(-4.23543574001425E-6,0.00445973646869292,0.0600520305933898));
#8401=CARTESIAN_POINT('',(0.00391685859097665,0.00607956303297287,0.0598959793798127));
#8402=CARTESIAN_POINT('',(0.00554029535879261,0.00999910325696514,0.0597390813899988));
#8403=CARTESIAN_POINT('',(0.00392195799437461,0.0139131258340931,0.0598955175187662));
#8404=CARTESIAN_POINT('',(5.55403455442611E-6,0.015541099119747,0.0600520956964933));
#8405=CARTESIAN_POINT('',(-0.0039149404887588,0.0139224634434835,0.0598960985083079));
#8406=CARTESIAN_POINT('',(-0.00554222253988876,0.00999901026546572,0.0597389564762431));
#8407=CARTESIAN_POINT('',(-0.00391616935168617,0.00608149549465367,0.0598958978797615));
#8408=CARTESIAN_POINT('',(-0.005,0.01,0.059791303715507));
#8409=CARTESIAN_POINT('',(0.,0.03,0.));
#8410=CARTESIAN_POINT('',(0.,0.,0.));
#8411=CARTESIAN_POINT('',(0.061,0.,0.));
#8412=CARTESIAN_POINT('',(0.,0.029,0.));
#8413=CARTESIAN_POINT('',(0.,0.029,0.061));
#8414=CARTESIAN_POINT('',(-0.00391494265834519,0.0139224651131911,0.0608978018788975));
#8415=CARTESIAN_POINT('',(-0.00554222119578978,0.00999900968220688,0.060743253346584));
#8416=CARTESIAN_POINT('',(-0.00391617255849569,0.0060814961579814,0.0608976044204628));
#8417=CARTESIAN_POINT('',(-4.2288777227757E-6,0.0044597393228037,0.061051177490022));
#8418=CARTESIAN_POINT('',(0.00391684609381935,0.0060795509475003,0.0608976852590645));
#8419=CARTESIAN_POINT('',(0.00554029932935669,0.00999910932086652,0.0607433760647901));
#8420=CARTESIAN_POINT('',(0.00392195461275095,0.013913123234971,0.0608972303299854));
#8421=CARTESIAN_POINT('',(5.56769475100309E-6,0.0155410993401316,0.0610512416549246));
#8422=CARTESIAN_POINT('',(-0.00391494265834519,0.0139224651131911,0.0608978018788975));
#8423=CARTESIAN_POINT('',(-0.00554222119578978,0.00999900968220688,0.060743253346584));
#8424=CARTESIAN_POINT('',(-0.00391617255849569,0.0060814961579814,0.0608976044204628));
#8425=CARTESIAN_POINT('',(-0.005,0.01,0.0607947366142827));
#8426=CARTESIAN_POINT('',(0.,0.03,0.));
#8427=CARTESIAN_POINT('',(0.,0.03,0.));
#8428=CARTESIAN_POINT('',(0.,0.03,0.0635));
#8429=CARTESIAN_POINT('',(0.,0.,0.));
#8430=CARTESIAN_POINT('',(-0.0135975206449919,0.,0.0124363480647457));
#8431=CARTESIAN_POINT('',(-0.0135975206449919,0.,0.0139363480647457));
#8432=CARTESIAN_POINT('',(-0.00538454930157943,0.,0.0176227679351839));
#8433=CARTESIAN_POINT('',(-0.00538454930157943,0.,0.0191227679351839));
#8434=CARTESIAN_POINT('',(0.00427564662218917,0.,0.00232533458508421));
#8435=CARTESIAN_POINT('',(0.00427564662218917,0.,0.00382533458508421));
#8436=CARTESIAN_POINT('',(-0.00393732472122328,0.,-0.00286108528535397));
#8437=CARTESIAN_POINT('',(-0.00393732472122328,0.,-0.00136108528535397));
#8438=CARTESIAN_POINT('',(0.,0.029,0.));
#8439=CARTESIAN_POINT('',(0.,0.029,0.));
#8440=CARTESIAN_POINT('',(0.,0.029,0.0635));
#8441=CARTESIAN_POINT('',(0.,0.029,0.));
#8442=CARTESIAN_POINT('',(0.,0.001,0.));
#8443=CARTESIAN_POINT('',(-0.0135975206449919,0.001,0.0124363480647457));
#8444=CARTESIAN_POINT('',(-0.0135975206449919,0.001,0.0109363480647457));
#8445=CARTESIAN_POINT('',(-0.00538454930157943,0.001,0.0176227679351839));
#8446=CARTESIAN_POINT('',(-0.00538454930157943,0.001,0.0161227679351839));
#8447=CARTESIAN_POINT('',(0.00427564662218917,0.001,0.00232533458508421));
#8448=CARTESIAN_POINT('',(0.00427564662218917,0.001,0.000825334585084205));
#8449=CARTESIAN_POINT('',(-0.00393732472122328,0.001,-0.00286108528535397));
#8450=CARTESIAN_POINT('',(-0.00393732472122328,0.001,-0.00436108528535397));
#8451=CARTESIAN_POINT('',(2.32682891837997E-18,0.01,0.124));
#8452=CARTESIAN_POINT('',(-0.00393732472122328,-0.181103382636493,-0.00286108528535397));
#8453=CARTESIAN_POINT('',(0.00427564662218917,-0.181103382636493,0.00232533458508421));
#8454=CARTESIAN_POINT('',(-0.00538454930157943,-0.181103382636493,0.0176227679351839));
#8455=CARTESIAN_POINT('',(-0.0135975206449919,-0.181103382636493,0.0124363480647457));
#8456=CARTESIAN_POINT('',(0.132889710102238,-0.0594770446550228,0.263382537537013));
#8457=CARTESIAN_POINT('',(-0.00104626020282667,0.,6.50521303491303E-19));
#8458=CARTESIAN_POINT('',(0.,-0.0003,6.50521303491303E-19));
#8459=CARTESIAN_POINT('',(-0.00197826943066075,-0.0003,6.50521303491303E-19));
#8460=CARTESIAN_POINT('',(0.00197826943066075,-0.0003,6.50521303491303E-19));
#8461=CARTESIAN_POINT('',(0.,0.,6.50521303491303E-19));
#8462=CARTESIAN_POINT('',(0.,0.,-0.0001));
#8463=CARTESIAN_POINT('',(0.,0.,-9.12844257252368E-5));
#8464=CARTESIAN_POINT('',(-0.00207897297737586,0.0003,-9.12844257252367E-5));
#8465=CARTESIAN_POINT('',(0.00207897297737584,0.0003,-9.12844257252368E-5));
#8466=CARTESIAN_POINT('',(-0.00207897297737584,0.0003,-9.12844257252392E-5));
#8467=CARTESIAN_POINT('',(-0.00207459712624839,0.0003,-4.17809699915527E-5));
#8468=CARTESIAN_POINT('',(-0.00202837661239549,0.0003,-6.48859435981983E-19));
#8469=CARTESIAN_POINT('',(-0.00197826943066076,0.0003,3.05634754505891E-21));
#8470=CARTESIAN_POINT('',(-0.00197826943066075,0.0003,6.50521303491303E-19));
#8471=CARTESIAN_POINT('',(0.,0.,6.50521303491303E-19));
#8472=CARTESIAN_POINT('',(0.00197826943066075,0.0003,6.50521303491303E-19));
#8473=CARTESIAN_POINT('',(0.00197826943066076,0.0003,1.75840007344507E-18));
#8474=CARTESIAN_POINT('',(0.00202795255984864,0.0003,1.11200139422846E-18));
#8475=CARTESIAN_POINT('',(0.00207460838288334,0.0003,-4.19083148928644E-5));
#8476=CARTESIAN_POINT('',(0.00207897297737584,0.0003,-9.12844257252363E-5));
#8477=CARTESIAN_POINT('',(0.,0.,-0.0059));
#8478=CARTESIAN_POINT('',(0.,0.,-0.01155643035625));
#8479=CARTESIAN_POINT('',(0.00125,0.,-0.01155643035625));
#8480=CARTESIAN_POINT('',(0.,0.,-0.0019));
#8481=CARTESIAN_POINT('',(-0.00125,0.,-0.0019));
#8482=CARTESIAN_POINT('',(-0.000625,0.,-0.0118));
#8483=CARTESIAN_POINT('',(0.,0.,-0.0118));
#8484=CARTESIAN_POINT('',(0.00100643035625,0.,-0.0118));
#8485=CARTESIAN_POINT('',(-0.00104626020282667,0.,6.50521303491303E-19));
#8486=CARTESIAN_POINT('',(-5.01008275896316E-5,0.0003,6.50521303491303E-19));
#8487=CARTESIAN_POINT('',(0.,0.,1.7347234759768E-18));
#8488=CARTESIAN_POINT('',(0.,0.,-9.12844257252368E-5));
#8489=CARTESIAN_POINT('',(0.00207897297737919,-0.0003,-9.12844257253807E-5));
#8490=CARTESIAN_POINT('',(-0.00207897297737586,-0.0003,-9.12844257252367E-5));
#8491=CARTESIAN_POINT('',(-0.00207897297737588,-0.0003,-9.12844257252345E-5));
#8492=CARTESIAN_POINT('',(-0.00209690871796292,-0.0003,-0.000294189212551693));
#8493=CARTESIAN_POINT('',(-0.00211483976375729,-0.0003,-0.000497094414503251));
#8494=CARTESIAN_POINT('',(-0.00213276646112605,-0.0003,-0.000699999999999993));
#8495=CARTESIAN_POINT('',(-0.00213276646112597,-0.0003,-0.0007));
#8496=CARTESIAN_POINT('',(0.,0.,-0.0007));
#8497=CARTESIAN_POINT('',(-0.00213276646112597,0.0003,-0.0007));
#8498=CARTESIAN_POINT('',(-0.00207897297737588,0.0003,-9.12844257252349E-5));
#8499=CARTESIAN_POINT('',(-0.00209690871796292,0.0003,-0.000294189212551693));
#8500=CARTESIAN_POINT('',(-0.00211483976375729,0.0003,-0.000497094414503251));
#8501=CARTESIAN_POINT('',(-0.00213276646112605,0.0003,-0.000699999999999993));
#8502=CARTESIAN_POINT('',(0.00213276646112605,0.0003,-0.000699999999999993));
#8503=CARTESIAN_POINT('',(0.00211483976374573,0.0003,-0.000497094414372398));
#8504=CARTESIAN_POINT('',(0.00209690871792154,0.0003,-0.000294189212083583));
#8505=CARTESIAN_POINT('',(0.00207897297737588,0.0003,-9.12844257252331E-5));
#8506=CARTESIAN_POINT('',(0.00213276646112597,0.0003,-0.0007));
#8507=CARTESIAN_POINT('',(0.,0.,-0.0007));
#8508=CARTESIAN_POINT('',(0.00213276646112597,-0.0003,-0.0007));
#8509=CARTESIAN_POINT('',(0.00213276646112605,-0.0003,-0.000699999999999993));
#8510=CARTESIAN_POINT('',(0.00211483976374574,-0.0003,-0.000497094414372544));
#8511=CARTESIAN_POINT('',(0.00209690871792157,-0.0003,-0.000294189212083876));
#8512=CARTESIAN_POINT('',(0.00207897297737592,-0.0003,-9.12844257256711E-5));
#8513=CARTESIAN_POINT('',(0.,0.,-0.0018));
#8514=CARTESIAN_POINT('',(-0.00225,0.,-0.0018));
#8515=CARTESIAN_POINT('',(-0.0018,0.,-0.0018));
#8516=CARTESIAN_POINT('',(0.,0.,-0.0018));
#8517=CARTESIAN_POINT('',(-0.00135,0.,-0.0018));
#8518=CARTESIAN_POINT('',(0.,0.,-0.0019));
#8519=CARTESIAN_POINT('',(0.,0.,-0.0001));
#8520=CARTESIAN_POINT('',(-0.00207897297737584,-0.0003,-9.12844257252392E-5));
#8521=CARTESIAN_POINT('',(-0.00207459712624839,-0.0003,-4.17809699915526E-5));
#8522=CARTESIAN_POINT('',(-0.00202837661239549,-0.0003,-6.54219152761022E-19));
#8523=CARTESIAN_POINT('',(-0.00197826943066076,-0.0003,-2.30336923397844E-21));
#8524=CARTESIAN_POINT('',(0.00197826943066075,-0.0003,1.76771743586486E-18));
#8525=CARTESIAN_POINT('',(0.00202795255984883,-0.0003,1.12131875664574E-18));
#8526=CARTESIAN_POINT('',(0.00207460838288366,-0.0003,-4.19083148932107E-5));
#8527=CARTESIAN_POINT('',(0.00207897297737589,-0.0003,-9.12844257258122E-5));
#8528=CARTESIAN_POINT('',(0.,0.,-0.0007));
#8529=CARTESIAN_POINT('',(0.,-0.0003,-0.0007));
#8530=CARTESIAN_POINT('',(-5.01008275896316E-5,0.0003,-0.0007));
#8531=CARTESIAN_POINT('',(0.,-0.0003,-0.0007));
#8532=CARTESIAN_POINT('',(-5.01008275896316E-5,0.0003,-0.0007));
#8533=CARTESIAN_POINT('',(0.,0.,-0.0118));
#8534=CARTESIAN_POINT('',(0.129859106257756,-0.0673818480688676,0.285367574957512));
#8535=CARTESIAN_POINT('',(0.132889710102238,-0.0594770446550229,0.287867574957512));
#8536=CARTESIAN_POINT('',(0.0151554445662277,0.002,0.00875));
#8537=CARTESIAN_POINT('',(0.0151554445662277,0.,0.00875));
#8538=CARTESIAN_POINT('',(0.0151554445662277,0.,-0.00375));
#8539=CARTESIAN_POINT('',(0.0141805044897511,0.,-0.00371192167553948));
#8540=CARTESIAN_POINT('',(0.0141805044897511,-0.0005,-0.00371192167553948));
#8541=CARTESIAN_POINT('',(0.0141805044897511,0.002,-0.00371192167553948));
#8542=CARTESIAN_POINT('',(0.0151554445662277,0.002,0.00875));
#8543=CARTESIAN_POINT('',(0.0151554445662277,0.002,-0.00375));
#8544=CARTESIAN_POINT('',(0.0151554445662277,0.002,-0.00375));
#8545=CARTESIAN_POINT('',(0.0151554445662277,0.002,0.00875));
#8546=CARTESIAN_POINT('',(0.0151554445662277,0.002,0.00875));
#8547=CARTESIAN_POINT('',(0.00269352289068823,0.002,0.00777505992352337));
#8548=CARTESIAN_POINT('',(0.00265544456622767,0.002,0.00875));
#8549=CARTESIAN_POINT('',(0.00269352289068823,-0.000499999999999958,0.00777505992352337));
#8550=CARTESIAN_POINT('',(0.00269352289068823,0.,0.00777505992352337));
#8551=CARTESIAN_POINT('',(0.0151554445662277,0.,0.00875));
#8552=CARTESIAN_POINT('',(0.00265544456622767,0.,0.00875));
#8553=CARTESIAN_POINT('',(0.00265544456622767,0.002,0.00875));
#8554=CARTESIAN_POINT('',(0.0151554445662277,0.002,0.00875));
#8555=CARTESIAN_POINT('',(0.0151554445662277,0.,0.00875));
#8556=CARTESIAN_POINT('',(0.0151554445662277,0.,0.01025));
#8557=CARTESIAN_POINT('',(0.0151554445662277,0.002,0.00875));
#8558=CARTESIAN_POINT('',(0.0151554445662277,0.002,0.01025));
#8559=CARTESIAN_POINT('',(0.0477117510540525,0.002,-0.0177067054013465));
#8560=CARTESIAN_POINT('',(0.0320811989597626,0.002,0.0191786316782243));
#8561=CARTESIAN_POINT('',(0.0320811989597626,0.002,0.0191786316782243));
#8562=CARTESIAN_POINT('',(0.0449321327792465,0.002,0.0191786316782244));
#8563=CARTESIAN_POINT('',(0.0320811989597626,0.002,0.0176786316782244));
#8564=CARTESIAN_POINT('',(0.0320811989597626,0.002,0.0161786316782242));
#8565=CARTESIAN_POINT('',(0.0320811989597626,0.002,0.0161786316782242));
#8566=CARTESIAN_POINT('',(0.0449321327792465,0.002,0.0161786316782242));
#8567=CARTESIAN_POINT('',(0.0449321327792465,0.002,0.0176786316782244));
#8568=CARTESIAN_POINT('',(0.0186533102025936,0.002,-0.00197008096664466));
#8569=CARTESIAN_POINT('',(0.0138888686280741,0.002,-0.00255325888374197));
#8570=CARTESIAN_POINT('',(0.0151554445662277,0.00200000000000005,0.00875));
#8571=CARTESIAN_POINT('',(0.0134533643050099,0.002,-0.00249592365190046));
#8572=CARTESIAN_POINT('',(0.00900220469196413,0.002,-0.000699488821690833));
#8573=CARTESIAN_POINT('',(0.0128717816969752,0.002,-0.00353962505122098));
#8574=CARTESIAN_POINT('',(0.0151554445662277,0.002,0.00875));
#8575=CARTESIAN_POINT('',(0.0125622380532049,0.002,-0.00347805299223131));
#8576=CARTESIAN_POINT('',(0.017224134128312,0.002,-0.00233493227030325));
#8577=CARTESIAN_POINT('',(0.0124243330190333,0.002,-0.00229123660269913));
#8578=CARTESIAN_POINT('',(0.0151554445662277,0.00200000000000005,0.00875));
#8579=CARTESIAN_POINT('',(0.0120000382453175,0.002,-0.00217754716072923));
#8580=CARTESIAN_POINT('',(0.0078214407177674,0.002,0.000184511835729573));
#8581=CARTESIAN_POINT('',(0.0112872007876491,0.002,-0.00313640778660604));
#8582=CARTESIAN_POINT('',(0.0151554445662277,0.002,0.00875));
#8583=CARTESIAN_POINT('',(0.0109883420990692,0.002,-0.00303495893196928));
#8584=CARTESIAN_POINT('',(0.0157595622020739,0.002,-0.00251011730949313));
#8585=CARTESIAN_POINT('',(0.0110065274857722,0.002,-0.00184029570217498));
#8586=CARTESIAN_POINT('',(0.0151554445662277,0.00200000000000005,0.00875));
#8587=CARTESIAN_POINT('',(0.0106007020626198,0.002,-0.00167219730794948));
#8588=CARTESIAN_POINT('',(0.00676616358278785,0.002,0.00121507037044262));
#8589=CARTESIAN_POINT('',(0.00976880660185426,0.002,-0.00252981078922743));
#8590=CARTESIAN_POINT('',(0.0151554445662277,0.002,0.00875));
#8591=CARTESIAN_POINT('',(0.00948574642348564,0.002,-0.00239022095697335));
#8592=CARTESIAN_POINT('',(0.0142846536555935,0.002,-0.00249263861962324));
#8593=CARTESIAN_POINT('',(0.00965971107405478,0.002,-0.00120815190600194));
#8594=CARTESIAN_POINT('',(0.0151554445662277,0.00200000000000005,0.00875));
#8595=CARTESIAN_POINT('',(0.0092792987869721,0.002,-0.000988520769651722));
#8596=CARTESIAN_POINT('',(0.00585442937138308,0.00200000000000003,0.00237455364019456));
#8597=CARTESIAN_POINT('',(0.00834257928508805,0.002,-0.00173021310189077));
#8598=CARTESIAN_POINT('',(0.0151554445662277,0.002,0.00875));
#8599=CARTESIAN_POINT('',(0.0080801608550617,0.002,-0.00155487071275084));
#8600=CARTESIAN_POINT('',(0.0128246445830229,0.002,-0.00228279526592331));
#8601=CARTESIAN_POINT('',(0.00840692818609363,0.002,-0.000405621369795907));
#8602=CARTESIAN_POINT('',(0.0151554445662277,0.00200000000000005,0.00875));
#8603=CARTESIAN_POINT('',(0.00805843799478281,0.002,-0.000138215440957164));
#8604=CARTESIAN_POINT('',(0.00510183810869068,0.00200000000000003,0.00364312256477043));
#8605=CARTESIAN_POINT('',(0.00703292198216526,0.002,-0.00075129606271674));
#8606=CARTESIAN_POINT('',(0.0151554445662277,0.002,0.00875));
#8607=CARTESIAN_POINT('',(0.00679563535257506,0.002,-0.000543201273583248));
#8608=CARTESIAN_POINT('',(0.0114045161443848,0.002,-0.00188417772635469));
#8609=CARTESIAN_POINT('',(0.0072696142844388,0.002,0.000553564386465146));
#8610=CARTESIAN_POINT('',(0.0151554445662277,0.00200000000000005,0.00875));
#8611=CARTESIAN_POINT('',(0.0069590089526929,0.002,0.000864169718211046));
#8612=CARTESIAN_POINT('',(0.00452126683987305,0.00200000000000004,0.00499907157815701));
#8613=CARTESIAN_POINT('',(0.00586224329264449,0.002,0.000390190786347311));
#8614=CARTESIAN_POINT('',(0.0151554445662277,0.002,0.00875));
#8615=CARTESIAN_POINT('',(0.005654148503511,0.002,0.000627477415937518));
#8616=CARTESIAN_POINT('',(0.0100485671309982,0.002,-0.00130360645753706));
#8617=CARTESIAN_POINT('',(0.00626722912527059,0.002,0.00165299342855505));
#8618=CARTESIAN_POINT('',(0.0151554445662277,0.00200000000000005,0.00875));
#8619=CARTESIAN_POINT('',(0.00599982319643184,0.002,0.00200148361986587));
#8620=CARTESIAN_POINT('',(0.00412264930030442,0.00200000000000004,0.00641920001679515));
#8621=CARTESIAN_POINT('',(0.00485057385347689,0.002,0.00167471628883397));
#8622=CARTESIAN_POINT('',(0.0151554445662277,0.002,0.00875));
#8623=CARTESIAN_POINT('',(0.00467523146433696,0.002,0.00193713471886032));
#8624=CARTESIAN_POINT('',(0.00877999820642231,0.002,-0.000551015194844674));
#8625=CARTESIAN_POINT('',(0.00541692379657602,0.002,0.00287385422074434));
#8626=CARTESIAN_POINT('',(0.0151554445662277,0.00200000000000005,0.00875));
#8627=CARTESIAN_POINT('',(0.0051972926602258,0.002,0.00325426650782702));
#8628=CARTESIAN_POINT('',(0.00391280594660448,0.00200000000000004,0.00787920908936577));
#8629=CARTESIAN_POINT('',(0.00401522360925438,0.002,0.0030803018572579));
#8630=CARTESIAN_POINT('',(0.0151554445662277,0.002,0.00875));
#8631=CARTESIAN_POINT('',(0.00387563377700029,0.002,0.0033633620356265));
#8632=CARTESIAN_POINT('',(0.00762051493667037,0.002,0.000360719016560104));
#8633=CARTESIAN_POINT('',(0.00473324725827826,0.002,0.00419525749639209));
#8634=CARTESIAN_POINT('',(0.0151554445662277,0.00200000000000005,0.00875));
#8635=CARTESIAN_POINT('',(0.00456514886405276,0.002,0.00460108291954443));
#8636=CARTESIAN_POINT('',(0.0038953272567346,0.00200000000000005,0.00935411763584619));
#8637=CARTESIAN_POINT('',(0.00337048563425844,0.002,0.00458289753284146));
#8638=CARTESIAN_POINT('',(0.0151554445662277,0.002,0.00875));
#8639=CARTESIAN_POINT('',(0.00326903677962168,0.002,0.00488175622142132));
#8640=CARTESIAN_POINT('',(0.00658995640195732,0.002,0.00141599615153965));
#8641=CARTESIAN_POINT('',(0.0042278974054985,0.002,0.00559459367908977));
#8642=CARTESIAN_POINT('',(0.0151554445662277,0.00200000000000005,0.00875));
#8643=CARTESIAN_POINT('',(0.00411420796352861,0.002,0.00601888845280556));
#8644=CARTESIAN_POINT('',(0.00407051229592446,0.00200000000000005,0.0108186895620842));
#8645=CARTESIAN_POINT('',(0.00292739157399641,0.002,0.00615679348697717));
#8646=CARTESIAN_POINT('',(0.0151554445662277,0.002,0.00875));
#8647=CARTESIAN_POINT('',(0.00286581951500674,0.002,0.00646633713074741));
#8648=CARTESIAN_POINT('',(0.00570595574453691,0.00200000000000003,0.00259676012573636));
#8649=CARTESIAN_POINT('',(0.00390952091432728,0.002,0.00704791973878213));
#8650=CARTESIAN_POINT('',(0.0151554445662277,0.00200000000000005,0.00875));
#8651=CARTESIAN_POINT('',(0.00385218568248577,0.002,0.00748342406184637));
#8652=CARTESIAN_POINT('',(0.00443536359958305,0.00200000000000006,0.0122478656363659));
#8653=CARTESIAN_POINT('',(0.00265544456622766,0.002,0.00875));
#8654=CARTESIAN_POINT('',(0.0226789374388172,0.002,0.0203105690001062));
#8655=CARTESIAN_POINT('',(0.0301789374388172,0.002,0.00732018794333958));
#8656=CARTESIAN_POINT('',(0.0301789374388172,0.002,0.0223201879433396));
#8657=CARTESIAN_POINT('',(0.0482520634848371,0.002,0.0223201879433396));
#8658=CARTESIAN_POINT('',(0.0482520634848371,0.002,0.0223201879433396));
#8659=CARTESIAN_POINT('',(0.046393043464028,0.002,0.0176786316782243));
#8660=CARTESIAN_POINT('',(0.0482520634848371,0.002,0.0130370754131091));
#8661=CARTESIAN_POINT('',(0.0482520634848371,0.002,0.0130370754131092));
#8662=CARTESIAN_POINT('',(0.0315024131220503,0.002,0.0130370754131092));
#8663=CARTESIAN_POINT('',(0.0315024131220503,0.002,0.00803707541310922));
#8664=CARTESIAN_POINT('',(0.0288383125530301,0.002,0.0122682180670677));
#8665=CARTESIAN_POINT('',(0.0477117510540525,0.002,-0.0177067054013465));
#8666=CARTESIAN_POINT('',(0.0477117510540525,0.,-0.0177067054013465));
#8667=CARTESIAN_POINT('',(0.0186533102025936,0.,-0.00197008096664465));
#8668=CARTESIAN_POINT('',(0.0138888686280741,0.,-0.00255325888374196));
#8669=CARTESIAN_POINT('',(0.0477117510540525,0.,-0.0177067054013465));
#8670=CARTESIAN_POINT('',(0.0288383125530301,0.,0.0122682180670677));
#8671=CARTESIAN_POINT('',(0.0315024131220503,0.,0.00803707541310922));
#8672=CARTESIAN_POINT('',(0.0315024131220503,0.,0.0130370754131092));
#8673=CARTESIAN_POINT('',(0.0482520634848371,0.,0.0130370754131092));
#8674=CARTESIAN_POINT('',(0.0482520634848371,0.,0.0130370754131091));
#8675=CARTESIAN_POINT('',(0.046393043464028,0.,0.0176786316782243));
#8676=CARTESIAN_POINT('',(0.0482520634848371,0.,0.0223201879433396));
#8677=CARTESIAN_POINT('',(0.0482520634848371,0.,0.0223201879433396));
#8678=CARTESIAN_POINT('',(0.0301789374388172,0.,0.0223201879433396));
#8679=CARTESIAN_POINT('',(0.0301789374388172,0.,0.00732018794333958));
#8680=CARTESIAN_POINT('',(0.0226789374388172,0.,0.0203105690001062));
#8681=CARTESIAN_POINT('',(0.00265544456622766,0.,0.00875));
#8682=CARTESIAN_POINT('',(0.00443536359958305,0.,0.0122478656363659));
#8683=CARTESIAN_POINT('',(0.00385218568248577,0.,0.00748342406184638));
#8684=CARTESIAN_POINT('',(0.0151554445662277,0.,0.00875));
#8685=CARTESIAN_POINT('',(0.00390952091432728,0.,0.00704791973878214));
#8686=CARTESIAN_POINT('',(0.00570595574453691,0.,0.00259676012573637));
#8687=CARTESIAN_POINT('',(0.00286581951500674,0.,0.00646633713074741));
#8688=CARTESIAN_POINT('',(0.0151554445662277,0.,0.00875));
#8689=CARTESIAN_POINT('',(0.00292739157399641,0.,0.00615679348697717));
#8690=CARTESIAN_POINT('',(0.00407051229592446,0.,0.0108186895620842));
#8691=CARTESIAN_POINT('',(0.00411420796352861,0.,0.00601888845280557));
#8692=CARTESIAN_POINT('',(0.0151554445662277,0.,0.00875));
#8693=CARTESIAN_POINT('',(0.0042278974054985,0.,0.00559459367908978));
#8694=CARTESIAN_POINT('',(0.00658995640195732,0.,0.00141599615153966));
#8695=CARTESIAN_POINT('',(0.00326903677962168,0.,0.00488175622142132));
#8696=CARTESIAN_POINT('',(0.0151554445662277,0.,0.00875));
#8697=CARTESIAN_POINT('',(0.00337048563425844,0.,0.00458289753284146));
#8698=CARTESIAN_POINT('',(0.0038953272567346,0.,0.00935411763584619));
#8699=CARTESIAN_POINT('',(0.00456514886405276,0.,0.00460108291954444));
#8700=CARTESIAN_POINT('',(0.0151554445662277,0.,0.00875));
#8701=CARTESIAN_POINT('',(0.00473324725827826,0.,0.0041952574963921));
#8702=CARTESIAN_POINT('',(0.00762051493667037,0.,0.000360719016560111));
#8703=CARTESIAN_POINT('',(0.00387563377700029,0.,0.0033633620356265));
#8704=CARTESIAN_POINT('',(0.0151554445662277,0.,0.00875));
#8705=CARTESIAN_POINT('',(0.00401522360925438,0.,0.0030803018572579));
#8706=CARTESIAN_POINT('',(0.00391280594660448,0.,0.00787920908936577));
#8707=CARTESIAN_POINT('',(0.0051972926602258,0.,0.00325426650782703));
#8708=CARTESIAN_POINT('',(0.0151554445662277,0.,0.00875));
#8709=CARTESIAN_POINT('',(0.00541692379657602,0.,0.00287385422074435));
#8710=CARTESIAN_POINT('',(0.00877999820642231,0.,-0.000551015194844667));
#8711=CARTESIAN_POINT('',(0.00467523146433696,0.,0.00193713471886032));
#8712=CARTESIAN_POINT('',(0.0151554445662277,0.,0.00875));
#8713=CARTESIAN_POINT('',(0.00485057385347689,0.,0.00167471628883397));
#8714=CARTESIAN_POINT('',(0.00412264930030442,0.,0.00641920001679516));
#8715=CARTESIAN_POINT('',(0.00599982319643184,0.,0.00200148361986588));
#8716=CARTESIAN_POINT('',(0.0151554445662277,0.,0.00875));
#8717=CARTESIAN_POINT('',(0.00626722912527059,0.,0.00165299342855506));
#8718=CARTESIAN_POINT('',(0.0100485671309982,0.,-0.00130360645753706));
#8719=CARTESIAN_POINT('',(0.005654148503511,0.,0.000627477415937518));
#8720=CARTESIAN_POINT('',(0.0151554445662277,0.,0.00875));
#8721=CARTESIAN_POINT('',(0.00586224329264449,0.,0.000390190786347311));
#8722=CARTESIAN_POINT('',(0.00452126683987305,0.,0.00499907157815702));
#8723=CARTESIAN_POINT('',(0.0069590089526929,0.,0.000864169718211053));
#8724=CARTESIAN_POINT('',(0.0151554445662277,0.,0.00875));
#8725=CARTESIAN_POINT('',(0.0072696142844388,0.,0.000553564386465153));
#8726=CARTESIAN_POINT('',(0.0114045161443848,0.,-0.00188417772635469));
#8727=CARTESIAN_POINT('',(0.00679563535257506,0.,-0.000543201273583248));
#8728=CARTESIAN_POINT('',(0.0151554445662277,0.,0.00875));
#8729=CARTESIAN_POINT('',(0.00703292198216526,0.,-0.00075129606271674));
#8730=CARTESIAN_POINT('',(0.00510183810869068,0.,0.00364312256477044));
#8731=CARTESIAN_POINT('',(0.00805843799478281,0.,-0.000138215440957157));
#8732=CARTESIAN_POINT('',(0.0151554445662277,0.,0.00875));
#8733=CARTESIAN_POINT('',(0.00840692818609363,0.,-0.0004056213697959));
#8734=CARTESIAN_POINT('',(0.0128246445830229,0.,-0.0022827952659233));
#8735=CARTESIAN_POINT('',(0.0080801608550617,0.,-0.00155487071275084));
#8736=CARTESIAN_POINT('',(0.0151554445662277,0.,0.00875));
#8737=CARTESIAN_POINT('',(0.00834257928508805,0.,-0.00173021310189077));
#8738=CARTESIAN_POINT('',(0.00585442937138308,0.,0.00237455364019457));
#8739=CARTESIAN_POINT('',(0.0092792987869721,0.,-0.000988520769651714));
#8740=CARTESIAN_POINT('',(0.0151554445662277,0.,0.00875));
#8741=CARTESIAN_POINT('',(0.00965971107405478,0.,-0.00120815190600194));
#8742=CARTESIAN_POINT('',(0.0142846536555935,0.,-0.00249263861962324));
#8743=CARTESIAN_POINT('',(0.00948574642348564,0.,-0.00239022095697335));
#8744=CARTESIAN_POINT('',(0.0151554445662277,0.,0.00875));
#8745=CARTESIAN_POINT('',(0.00976880660185426,0.,-0.00252981078922743));
#8746=CARTESIAN_POINT('',(0.00676616358278785,0.,0.00121507037044262));
#8747=CARTESIAN_POINT('',(0.0106007020626198,0.,-0.00167219730794947));
#8748=CARTESIAN_POINT('',(0.0151554445662277,0.,0.00875));
#8749=CARTESIAN_POINT('',(0.0110065274857722,0.,-0.00184029570217498));
#8750=CARTESIAN_POINT('',(0.0157595622020739,0.,-0.00251011730949312));
#8751=CARTESIAN_POINT('',(0.0109883420990692,0.,-0.00303495893196928));
#8752=CARTESIAN_POINT('',(0.0151554445662277,0.,0.00875));
#8753=CARTESIAN_POINT('',(0.0112872007876491,0.,-0.00313640778660604));
#8754=CARTESIAN_POINT('',(0.0078214407177674,0.,0.00018451183572958));
#8755=CARTESIAN_POINT('',(0.0120000382453175,0.,-0.00217754716072922));
#8756=CARTESIAN_POINT('',(0.0151554445662277,0.,0.00875));
#8757=CARTESIAN_POINT('',(0.0124243330190333,0.,-0.00229123660269911));
#8758=CARTESIAN_POINT('',(0.017224134128312,0.,-0.00233493227030325));
#8759=CARTESIAN_POINT('',(0.0125622380532049,0.,-0.00347805299223131));
#8760=CARTESIAN_POINT('',(0.0151554445662277,0.,0.00875));
#8761=CARTESIAN_POINT('',(0.0128717816969752,0.,-0.00353962505122098));
#8762=CARTESIAN_POINT('',(0.00900220469196413,0.,-0.000699488821690826));
#8763=CARTESIAN_POINT('',(0.0134533643050099,0.,-0.00249592365190045));
#8764=CARTESIAN_POINT('',(0.0151554445662277,0.,0.00875));
#8765=CARTESIAN_POINT('',(0.0320811989597626,0.,0.0176786316782244));
#8766=CARTESIAN_POINT('',(0.0320811989597626,0.,0.0161786316782242));
#8767=CARTESIAN_POINT('',(0.0320811989597626,0.,0.0191786316782243));
#8768=CARTESIAN_POINT('',(0.0320811989597626,0.,0.0191786316782243));
#8769=CARTESIAN_POINT('',(0.0449321327792465,0.,0.0191786316782244));
#8770=CARTESIAN_POINT('',(0.0449321327792465,0.,0.0176786316782244));
#8771=CARTESIAN_POINT('',(0.0449321327792465,0.,0.0161786316782242));
#8772=CARTESIAN_POINT('',(0.0320811989597626,0.,0.0161786316782242));
#8773=CARTESIAN_POINT('',(0.00265544456622766,0.002,0.00875));
#8774=CARTESIAN_POINT('',(0.0226789374388172,0.002,0.0203105690001062));
#8775=CARTESIAN_POINT('',(0.0477117510540525,0.002,-0.0177067054013465));
#8776=CARTESIAN_POINT('',(0.0288383125530301,0.002,0.0122682180670677));
#8777=CARTESIAN_POINT('',(0.0315024131220503,0.002,0.00803707541310922));
#8778=CARTESIAN_POINT('',(0.0315024131220503,0.002,0.0130370754131092));
#8779=CARTESIAN_POINT('',(0.0482520634848371,0.002,0.0130370754131092));
#8780=CARTESIAN_POINT('',(0.0482520634848371,0.002,0.0130370754131091));
#8781=CARTESIAN_POINT('',(0.046393043464028,0.002,0.0176786316782243));
#8782=CARTESIAN_POINT('',(0.0482520634848371,0.002,0.0223201879433396));
#8783=CARTESIAN_POINT('',(0.0482520634848371,0.002,0.0223201879433396));
#8784=CARTESIAN_POINT('',(0.0301789374388172,0.002,0.0223201879433396));
#8785=CARTESIAN_POINT('',(0.0301789374388172,0.002,0.00732018794333958));
#8786=CARTESIAN_POINT('',(0.0320811989597626,0.002,0.0176786316782244));
#8787=CARTESIAN_POINT('',(0.0320811989597626,0.002,0.0161786316782242));
#8788=CARTESIAN_POINT('',(0.0320811989597626,0.002,0.0191786316782243));
#8789=CARTESIAN_POINT('',(0.0320811989597626,0.002,0.0191786316782243));
#8790=CARTESIAN_POINT('',(0.0449321327792465,0.002,0.0191786316782244));
#8791=CARTESIAN_POINT('',(0.0449321327792465,0.002,0.0176786316782244));
#8792=CARTESIAN_POINT('',(0.0449321327792465,0.002,0.0161786316782242));
#8793=CARTESIAN_POINT('',(0.0320811989597626,0.002,0.0161786316782242));
#8794=CARTESIAN_POINT('',(0.0151554445662277,0.002,0.00875));
#8795=CARTESIAN_POINT('',(0.00292739157399641,-0.000499999999999964,0.00615679348697716));
#8796=CARTESIAN_POINT('',(0.00286581951500674,-0.000499999999999964,0.00646633713074741));
#8797=CARTESIAN_POINT('',(0.0151554445662277,0.002,0.00875));
#8798=CARTESIAN_POINT('',(0.00337048563425845,-0.000499999999999969,0.00458289753284145));
#8799=CARTESIAN_POINT('',(0.00326903677962168,-0.000499999999999969,0.00488175622142132));
#8800=CARTESIAN_POINT('',(0.0151554445662277,0.002,0.00875));
#8801=CARTESIAN_POINT('',(0.00387563377700029,-0.000499999999999973,0.0033633620356265));
#8802=CARTESIAN_POINT('',(0.00401522360925438,-0.000499999999999975,0.0030803018572579));
#8803=CARTESIAN_POINT('',(0.0151554445662277,0.002,0.00875));
#8804=CARTESIAN_POINT('',(0.00467523146433696,-0.000499999999999979,0.00193713471886031));
#8805=CARTESIAN_POINT('',(0.00485057385347689,-0.00049999999999998,0.00167471628883396));
#8806=CARTESIAN_POINT('',(0.0151554445662277,0.002,0.00875));
#8807=CARTESIAN_POINT('',(0.00586224329264449,-0.000499999999999983,0.000390190786347312));
#8808=CARTESIAN_POINT('',(0.005654148503511,-0.000499999999999982,0.000627477415937519));
#8809=CARTESIAN_POINT('',(0.0151554445662277,0.002,0.00875));
#8810=CARTESIAN_POINT('',(0.00703292198216527,-0.000499999999999989,-0.000751296062716742));
#8811=CARTESIAN_POINT('',(0.00679563535257506,-0.000499999999999986,-0.000543201273583248));
#8812=CARTESIAN_POINT('',(0.0151554445662277,0.002,0.00875));
#8813=CARTESIAN_POINT('',(0.00808016085506171,-0.00049999999999999,-0.00155487071275084));
#8814=CARTESIAN_POINT('',(0.00834257928508806,-0.000499999999999991,-0.00173021310189077));
#8815=CARTESIAN_POINT('',(0.0151554445662277,0.002,0.00875));
#8816=CARTESIAN_POINT('',(0.00976880660185426,-0.000499999999999994,-0.00252981078922743));
#8817=CARTESIAN_POINT('',(0.00948574642348565,-0.000499999999999994,-0.00239022095697335));
#8818=CARTESIAN_POINT('',(0.0151554445662277,0.002,0.00875));
#8819=CARTESIAN_POINT('',(0.0112872007876491,-0.0005,-0.00313640778660604));
#8820=CARTESIAN_POINT('',(0.0109883420990692,-0.0005,-0.00303495893196928));
#8821=CARTESIAN_POINT('',(0.0151554445662277,0.002,0.00875));
#8822=CARTESIAN_POINT('',(0.0128717816969752,-0.0005,-0.00353962505122098));
#8823=CARTESIAN_POINT('',(0.0125622380532049,-0.0005,-0.00347805299223131));
#8824=CARTESIAN_POINT('',(0.0186533102025936,0.002,-0.00197008096664466));
#8825=CARTESIAN_POINT('',(0.0138888686280741,0.002,-0.00255325888374197));
#8826=CARTESIAN_POINT('',(0.0151554445662277,0.00200000000000005,0.00875));
#8827=CARTESIAN_POINT('',(0.0134533643050099,0.002,-0.00249592365190045));
#8828=CARTESIAN_POINT('',(0.00900220469196413,0.002,-0.000699488821690833));
#8829=CARTESIAN_POINT('',(0.017224134128312,0.002,-0.00233493227030325));
#8830=CARTESIAN_POINT('',(0.0124243330190333,0.002,-0.00229123660269913));
#8831=CARTESIAN_POINT('',(0.0151554445662277,0.00200000000000005,0.00875));
#8832=CARTESIAN_POINT('',(0.0120000382453175,0.002,-0.00217754716072923));
#8833=CARTESIAN_POINT('',(0.0078214407177674,0.002,0.000184511835729573));
#8834=CARTESIAN_POINT('',(0.0157595622020739,0.002,-0.00251011730949313));
#8835=CARTESIAN_POINT('',(0.0110065274857722,0.002,-0.00184029570217498));
#8836=CARTESIAN_POINT('',(0.0151554445662277,0.00200000000000005,0.00875));
#8837=CARTESIAN_POINT('',(0.0106007020626198,0.002,-0.00167219730794948));
#8838=CARTESIAN_POINT('',(0.00676616358278785,0.002,0.00121507037044262));
#8839=CARTESIAN_POINT('',(0.0142846536555935,0.002,-0.00249263861962324));
#8840=CARTESIAN_POINT('',(0.00965971107405478,0.002,-0.00120815190600194));
#8841=CARTESIAN_POINT('',(0.0151554445662277,0.00200000000000005,0.00875));
#8842=CARTESIAN_POINT('',(0.0092792987869721,0.002,-0.000988520769651722));
#8843=CARTESIAN_POINT('',(0.00585442937138308,0.00200000000000003,0.00237455364019456));
#8844=CARTESIAN_POINT('',(0.0128246445830229,0.002,-0.00228279526592331));
#8845=CARTESIAN_POINT('',(0.00840692818609363,0.002,-0.000405621369795907));
#8846=CARTESIAN_POINT('',(0.0151554445662277,0.00200000000000005,0.00875));
#8847=CARTESIAN_POINT('',(0.00805843799478281,0.002,-0.000138215440957164));
#8848=CARTESIAN_POINT('',(0.00510183810869068,0.00200000000000003,0.00364312256477043));
#8849=CARTESIAN_POINT('',(0.0114045161443848,0.002,-0.00188417772635469));
#8850=CARTESIAN_POINT('',(0.0072696142844388,0.002,0.000553564386465144));
#8851=CARTESIAN_POINT('',(0.0151554445662277,0.00200000000000005,0.00875));
#8852=CARTESIAN_POINT('',(0.0069590089526929,0.002,0.000864169718211046));
#8853=CARTESIAN_POINT('',(0.00452126683987305,0.00200000000000004,0.00499907157815701));
#8854=CARTESIAN_POINT('',(0.0100485671309982,0.002,-0.00130360645753706));
#8855=CARTESIAN_POINT('',(0.00626722912527059,0.002,0.00165299342855505));
#8856=CARTESIAN_POINT('',(0.0151554445662277,0.00200000000000005,0.00875));
#8857=CARTESIAN_POINT('',(0.00599982319643184,0.00200000000000003,0.00200148361986588));
#8858=CARTESIAN_POINT('',(0.00412264930030442,0.00200000000000004,0.00641920001679515));
#8859=CARTESIAN_POINT('',(0.00877999820642231,0.002,-0.000551015194844674));
#8860=CARTESIAN_POINT('',(0.00541692379657602,0.00200000000000003,0.00287385422074434));
#8861=CARTESIAN_POINT('',(0.0151554445662277,0.00200000000000005,0.00875));
#8862=CARTESIAN_POINT('',(0.0051972926602258,0.00200000000000003,0.00325426650782702));
#8863=CARTESIAN_POINT('',(0.00391280594660448,0.00200000000000004,0.00787920908936577));
#8864=CARTESIAN_POINT('',(0.00762051493667037,0.002,0.000360719016560104));
#8865=CARTESIAN_POINT('',(0.00473324725827826,0.00200000000000003,0.00419525749639209));
#8866=CARTESIAN_POINT('',(0.0151554445662277,0.00200000000000005,0.00875));
#8867=CARTESIAN_POINT('',(0.00456514886405276,0.00200000000000003,0.00460108291954443));
#8868=CARTESIAN_POINT('',(0.0038953272567346,0.00200000000000005,0.00935411763584619));
#8869=CARTESIAN_POINT('',(0.00658995640195732,0.002,0.00141599615153965));
#8870=CARTESIAN_POINT('',(0.0042278974054985,0.00200000000000004,0.00559459367908977));
#8871=CARTESIAN_POINT('',(0.0151554445662277,0.00200000000000005,0.00875));
#8872=CARTESIAN_POINT('',(0.00411420796352861,0.00200000000000004,0.00601888845280556));
#8873=CARTESIAN_POINT('',(0.00407051229592446,0.00200000000000005,0.0108186895620842));
#8874=CARTESIAN_POINT('',(0.00570595574453691,0.00200000000000003,0.00259676012573636));
#8875=CARTESIAN_POINT('',(0.00390952091432728,0.00200000000000004,0.00704791973878213));
#8876=CARTESIAN_POINT('',(0.0151554445662277,0.00200000000000005,0.00875));
#8877=CARTESIAN_POINT('',(0.00385218568248577,0.00200000000000004,0.00748342406184637));
#8878=CARTESIAN_POINT('',(0.00443536359958305,0.00200000000000006,0.0122478656363659));
#8879=CARTESIAN_POINT('',(0.138477762351222,-0.0629232718347731,0.273067574957509));
#8880=CARTESIAN_POINT('',(0.126630475383547,-0.075803170572947,0.285367574957512));
#8881=CARTESIAN_POINT('',(-0.006,0.025,0.006));
#8882=CARTESIAN_POINT('',(-0.006,0.025,0.004));
#8883=CARTESIAN_POINT('',(-0.006,0.,0.004));
#8884=CARTESIAN_POINT('',(-0.006,0.0184403410758551,0.004));
#8885=CARTESIAN_POINT('',(-0.006,0.0184403410758551,0.006));
#8886=CARTESIAN_POINT('',(-0.006,0.0184403410758551,-0.004));
#8887=CARTESIAN_POINT('',(-0.006,0.025,-0.004));
#8888=CARTESIAN_POINT('',(-0.006,0.,-0.004));
#8889=CARTESIAN_POINT('',(-0.006,0.,0.006));
#8890=CARTESIAN_POINT('',(-0.006,0.025,0.006));
#8891=CARTESIAN_POINT('',(-0.006,0.025,-0.004));
#8892=CARTESIAN_POINT('',(-0.006,0.025,-0.004));
#8893=CARTESIAN_POINT('',(-0.006,0.0215596589241449,-0.004));
#8894=CARTESIAN_POINT('',(-0.006,0.0215596589241449,0.006));
#8895=CARTESIAN_POINT('',(-0.006,0.0215596589241449,0.004));
#8896=CARTESIAN_POINT('',(-0.006,0.025,0.004));
#8897=CARTESIAN_POINT('',(-0.006,0.025,0.004));
#8898=CARTESIAN_POINT('',(-0.006,0.025,0.006));
#8899=CARTESIAN_POINT('',(-0.006,0.025,0.));
#8900=CARTESIAN_POINT('',(-0.006,0.025,0.006));
#8901=CARTESIAN_POINT('',(-0.006,0.025,0.006));
#8902=CARTESIAN_POINT('',(-0.006,0.0184403410758551,0.006));
#8903=CARTESIAN_POINT('',(-0.004,0.0184403410758551,0.006));
#8904=CARTESIAN_POINT('',(0.004,0.0184403410758551,0.006));
#8905=CARTESIAN_POINT('',(-0.004,0.,0.006));
#8906=CARTESIAN_POINT('',(-0.004,0.0104638876866717,0.006));
#8907=CARTESIAN_POINT('',(-0.0025,0.00914101203113945,0.006));
#8908=CARTESIAN_POINT('',(-0.0025,0.0111410120311394,0.006));
#8909=CARTESIAN_POINT('',(-0.0025,0.0111410120311394,0.006));
#8910=CARTESIAN_POINT('',(0.0025,0.0111410120311394,0.006));
#8911=CARTESIAN_POINT('',(0.0025,0.00914101203113945,0.006));
#8912=CARTESIAN_POINT('',(0.004,0.0104638876866717,0.006));
#8913=CARTESIAN_POINT('',(0.004,0.025,0.006));
#8914=CARTESIAN_POINT('',(-0.006,0.025,0.006));
#8915=CARTESIAN_POINT('',(-0.006,0.0215596589241449,0.006));
#8916=CARTESIAN_POINT('',(0.004,0.0215596589241449,0.006));
#8917=CARTESIAN_POINT('',(-0.004,0.0215596589241449,0.006));
#8918=CARTESIAN_POINT('',(0.004,0.025,0.006));
#8919=CARTESIAN_POINT('',(0.004,0.025,0.006));
#8920=CARTESIAN_POINT('',(-0.006,0.025,0.006));
#8921=CARTESIAN_POINT('',(0.,0.025,0.006));
#8922=CARTESIAN_POINT('',(-0.006,0.025,0.006));
#8923=CARTESIAN_POINT('',(-0.004,0.025,0.006));
#8924=CARTESIAN_POINT('',(-0.004,0.,0.006));
#8925=CARTESIAN_POINT('',(0.006,0.025,0.006));
#8926=CARTESIAN_POINT('',(0.006,0.0184403410758551,0.006));
#8927=CARTESIAN_POINT('',(0.006,0.0184403410758551,0.004));
#8928=CARTESIAN_POINT('',(0.006,0.0184403410758551,-0.004));
#8929=CARTESIAN_POINT('',(0.006,0.025,0.004));
#8930=CARTESIAN_POINT('',(0.006,0.,0.004));
#8931=CARTESIAN_POINT('',(0.006,0.,0.006));
#8932=CARTESIAN_POINT('',(0.006,0.,-0.004));
#8933=CARTESIAN_POINT('',(0.006,0.025,-0.004));
#8934=CARTESIAN_POINT('',(0.006,0.025,0.006));
#8935=CARTESIAN_POINT('',(0.006,0.0215596589241449,0.006));
#8936=CARTESIAN_POINT('',(0.006,0.0215596589241449,-0.004));
#8937=CARTESIAN_POINT('',(0.006,0.0215596589241449,0.004));
#8938=CARTESIAN_POINT('',(0.006,0.025,-0.004));
#8939=CARTESIAN_POINT('',(0.006,0.025,-0.004));
#8940=CARTESIAN_POINT('',(0.006,0.025,0.006));
#8941=CARTESIAN_POINT('',(0.006,0.025,0.));
#8942=CARTESIAN_POINT('',(0.006,0.025,0.006));
#8943=CARTESIAN_POINT('',(0.006,0.025,0.004));
#8944=CARTESIAN_POINT('',(0.006,0.025,0.004));
#8945=CARTESIAN_POINT('',(-0.006,0.025,-0.006));
#8946=CARTESIAN_POINT('',(-0.004,0.025,-0.006));
#8947=CARTESIAN_POINT('',(-0.004,0.,-0.006));
#8948=CARTESIAN_POINT('',(-0.004,0.0184403410758551,-0.006));
#8949=CARTESIAN_POINT('',(-0.006,0.0184403410758551,-0.006));
#8950=CARTESIAN_POINT('',(0.004,0.0184403410758551,-0.006));
#8951=CARTESIAN_POINT('',(0.004,0.,-0.006));
#8952=CARTESIAN_POINT('',(0.004,0.,-0.006));
#8953=CARTESIAN_POINT('',(-0.006,0.,-0.006));
#8954=CARTESIAN_POINT('',(-0.006,0.025,-0.006));
#8955=CARTESIAN_POINT('',(0.004,0.,-0.006));
#8956=CARTESIAN_POINT('',(0.004,0.025,-0.006));
#8957=CARTESIAN_POINT('',(0.004,0.0215596589241449,-0.006));
#8958=CARTESIAN_POINT('',(-0.006,0.0215596589241449,-0.006));
#8959=CARTESIAN_POINT('',(-0.004,0.0215596589241449,-0.006));
#8960=CARTESIAN_POINT('',(-0.004,0.025,-0.006));
#8961=CARTESIAN_POINT('',(-0.004,0.025,-0.006));
#8962=CARTESIAN_POINT('',(-0.006,0.025,-0.006));
#8963=CARTESIAN_POINT('',(0.,0.025,-0.006));
#8964=CARTESIAN_POINT('',(-0.006,0.025,-0.006));
#8965=CARTESIAN_POINT('',(-0.004,0.025,0.004));
#8966=CARTESIAN_POINT('',(-0.004,0.0184403410758551,0.004));
#8967=CARTESIAN_POINT('',(-0.004,0.,0.004));
#8968=CARTESIAN_POINT('',(-0.004,0.,0.006));
#8969=CARTESIAN_POINT('',(-0.004,0.,0.006));
#8970=CARTESIAN_POINT('',(-0.004,0.00781813637560716,0.006));
#8971=CARTESIAN_POINT('',(-0.004,0.0104638876866717,0.006));
#8972=CARTESIAN_POINT('',(-0.00432213201520761,0.0100986243145697,0.006));
#8973=CARTESIAN_POINT('',(-0.00467795026178238,0.00914209250915622,0.00587298337765155));
#8974=CARTESIAN_POINT('',(-0.00432196721766239,0.0081832128848572,0.006));
#8975=CARTESIAN_POINT('',(-0.004,0.00781813637560716,0.006));
#8976=CARTESIAN_POINT('',(-0.004,0.025,0.004));
#8977=CARTESIAN_POINT('',(-0.004,0.0215596589241449,0.004));
#8978=CARTESIAN_POINT('',(-0.004,0.025,0.004));
#8979=CARTESIAN_POINT('',(-0.004,0.025,-0.004));
#8980=CARTESIAN_POINT('',(-0.004,0.0184403410758551,-0.004));
#8981=CARTESIAN_POINT('',(-0.004,0.,-0.004));
#8982=CARTESIAN_POINT('',(-0.004,0.025,-0.004));
#8983=CARTESIAN_POINT('',(-0.004,0.0215596589241449,-0.004));
#8984=CARTESIAN_POINT('',(-0.004,0.025,-0.004));
#8985=CARTESIAN_POINT('',(0.004,0.025,-0.004));
#8986=CARTESIAN_POINT('',(0.004,0.0184403410758551,-0.004));
#8987=CARTESIAN_POINT('',(0.004,0.,-0.004));
#8988=CARTESIAN_POINT('',(0.004,0.025,-0.004));
#8989=CARTESIAN_POINT('',(0.004,0.0215596589241449,-0.004));
#8990=CARTESIAN_POINT('',(0.004,0.025,-0.004));
#8991=CARTESIAN_POINT('',(0.004,0.025,0.004));
#8992=CARTESIAN_POINT('',(0.004,0.0184403410758551,0.004));
#8993=CARTESIAN_POINT('',(0.004,0.00781813637560717,0.006));
#8994=CARTESIAN_POINT('',(0.00432213201520761,0.0081833997477092,0.006));
#8995=CARTESIAN_POINT('',(0.00467795026178238,0.00913993155312269,0.00587298337765155));
#8996=CARTESIAN_POINT('',(0.00432196721766239,0.0100988111774217,0.006));
#8997=CARTESIAN_POINT('',(0.004,0.0104638876866717,0.006));
#8998=CARTESIAN_POINT('',(0.004,0.00781813637560717,0.006));
#8999=CARTESIAN_POINT('',(0.004,0.025,0.006));
#9000=CARTESIAN_POINT('',(0.004,0.,0.006));
#9001=CARTESIAN_POINT('',(0.004,0.,0.004));
#9002=CARTESIAN_POINT('',(0.004,0.025,0.004));
#9003=CARTESIAN_POINT('',(0.004,0.0215596589241449,0.004));
#9004=CARTESIAN_POINT('',(0.004,0.025,0.004));
#9005=CARTESIAN_POINT('',(-0.006,0.025,0.006));
#9006=CARTESIAN_POINT('',(-0.006,0.,0.006));
#9007=CARTESIAN_POINT('',(0.0025,0.00914101203113945,0.006));
#9008=CARTESIAN_POINT('',(0.0025,0.00714101203113945,0.006));
#9009=CARTESIAN_POINT('',(-0.0025,0.00714101203113946,0.006));
#9010=CARTESIAN_POINT('',(-0.0025,0.00714101203113946,0.006));
#9011=CARTESIAN_POINT('',(-0.0025,0.00914101203113945,0.006));
#9012=CARTESIAN_POINT('',(0.,0.025,0.));
#9013=CARTESIAN_POINT('',(0.,0.025,0.));
#9014=CARTESIAN_POINT('',(0.,0.025,0.));
#9015=CARTESIAN_POINT('',(0.,0.025,0.));
#9016=CARTESIAN_POINT('',(0.,0.025,0.));
#9017=CARTESIAN_POINT('',(0.,0.025,0.));
#9018=CARTESIAN_POINT('',(0.0025,0.0106410120311394,-0.0015));
#9019=CARTESIAN_POINT('',(0.0025,0.0106410120311394,0.001));
#9020=CARTESIAN_POINT('',(0.0025,0.0106410120311394,0.001));
#9021=CARTESIAN_POINT('',(0.00111803398874989,0.0106410120311394,0.001));
#9022=CARTESIAN_POINT('',(0.,0.0106410120311394,0.));
#9023=CARTESIAN_POINT('',(0.,0.0106410120311394,-0.0015));
#9024=CARTESIAN_POINT('',(0.0025,0.0106410120311394,-0.0015));
#9025=CARTESIAN_POINT('',(0.0025,0.0106410120311394,-0.0015));
#9026=CARTESIAN_POINT('',(0.0025,0.0106410120311394,-0.0015));
#9027=CARTESIAN_POINT('',(0.,0.025,0.));
#9028=CARTESIAN_POINT('',(0.,0.025,0.));
#9029=CARTESIAN_POINT('',(0.,0.,0.));
#9030=CARTESIAN_POINT('',(0.,0.038,0.));
#9031=CARTESIAN_POINT('',(0.,0.027,0.));
#9032=CARTESIAN_POINT('',(0.,0.027,-0.004));
#9033=CARTESIAN_POINT('',(0.,0.0365,0.));
#9034=CARTESIAN_POINT('',(0.,0.0365,0.004));
#9035=CARTESIAN_POINT('',(0.,0.038,0.));
#9036=CARTESIAN_POINT('',(0.,0.038,0.));
#9037=CARTESIAN_POINT('',(0.,0.038,0.0015));
#9038=CARTESIAN_POINT('',(0.,0.038,0.));
#9039=CARTESIAN_POINT('',(0.,0.038,0.0025));
#9040=CARTESIAN_POINT('',(0.,0.038,0.));
#9041=CARTESIAN_POINT('',(-0.0025,0.00914101203113945,0.001));
#9042=CARTESIAN_POINT('',(-0.0025,0.00714101203113946,0.001));
#9043=CARTESIAN_POINT('',(-0.0025,0.00714101203113946,0.001));
#9044=CARTESIAN_POINT('',(-0.0025,0.00914101203113945,0.001));
#9045=CARTESIAN_POINT('',(-0.0025,0.0111410120311394,0.001));
#9046=CARTESIAN_POINT('',(-0.0025,0.0111410120311394,0.001));
#9047=CARTESIAN_POINT('',(-0.0025,0.0111410120311394,0.001));
#9048=CARTESIAN_POINT('',(-0.0025,0.0111410120311394,0.001));
#9049=CARTESIAN_POINT('',(-0.00111803398874989,0.0111410120311394,0.001));
#9050=CARTESIAN_POINT('',(0.,0.0111410120311394,0.));
#9051=CARTESIAN_POINT('',(0.00111803398874989,0.0111410120311394,0.001));
#9052=CARTESIAN_POINT('',(-0.0025,0.0111410120311394,0.001));
#9053=CARTESIAN_POINT('',(0.0025,0.0111410120311394,0.001));
#9054=CARTESIAN_POINT('',(0.0025,0.0111410120311394,0.001));
#9055=CARTESIAN_POINT('',(0.0025,0.00914101203113945,0.001));
#9056=CARTESIAN_POINT('',(0.0025,0.00914101203113945,0.001));
#9057=CARTESIAN_POINT('',(0.0025,0.00714101203113945,0.001));
#9058=CARTESIAN_POINT('',(0.0025,0.00714101203113945,0.001));
#9059=CARTESIAN_POINT('',(-0.0025,0.00714101203113946,0.001));
#9060=CARTESIAN_POINT('',(-0.0025,0.00714101203113946,0.001));
#9061=CARTESIAN_POINT('',(-0.0025,0.00914101203113945,0.001));
#9062=CARTESIAN_POINT('',(0.00111803398874989,0.00639837134402017,0.001));
#9063=CARTESIAN_POINT('',(0.0025,0.00914101203113945,0.001));
#9064=CARTESIAN_POINT('',(0.0025,0.00764101203113946,0.001));
#9065=CARTESIAN_POINT('',(-0.0025,0.00764101203113946,0.001));
#9066=CARTESIAN_POINT('',(-0.0025,0.00764101203113946,0.001));
#9067=CARTESIAN_POINT('',(-0.0025,0.00914101203113945,0.001));
#9068=CARTESIAN_POINT('',(-0.0025,0.0106410120311394,0.001));
#9069=CARTESIAN_POINT('',(0.0025,0.0106410120311394,0.001));
#9070=CARTESIAN_POINT('',(-0.00111803398874989,0.0106410120311394,0.001));
#9071=CARTESIAN_POINT('',(-0.00111803398874989,0.00639837134402017,0.001));
#9072=CARTESIAN_POINT('',(-0.0025,0.00914101203113945,-0.0015));
#9073=CARTESIAN_POINT('',(-0.0025,0.00764101203113946,-0.0015));
#9074=CARTESIAN_POINT('',(-0.0025,0.00764101203113946,-0.0015));
#9075=CARTESIAN_POINT('',(-0.0025,0.00914101203113945,-0.0015));
#9076=CARTESIAN_POINT('',(-0.0025,0.0106410120311394,-0.0015));
#9077=CARTESIAN_POINT('',(-0.0025,0.0106410120311394,-0.0015));
#9078=CARTESIAN_POINT('',(0.0025,0.0106410120311394,-0.0015));
#9079=CARTESIAN_POINT('',(0.0025,0.0106410120311394,-0.0015));
#9080=CARTESIAN_POINT('',(0.,0.0106410120311394,0.));
#9081=CARTESIAN_POINT('',(0.0025,0.00914101203113945,-0.0015));
#9082=CARTESIAN_POINT('',(0.0025,0.00914101203113945,-0.0015));
#9083=CARTESIAN_POINT('',(0.0025,0.00764101203113946,-0.0015));
#9084=CARTESIAN_POINT('',(0.0025,0.00764101203113946,-0.0015));
#9085=CARTESIAN_POINT('',(-0.0025,0.00764101203113946,-0.0015));
#9086=CARTESIAN_POINT('',(-0.0025,0.00764101203113946,-0.0015));
#9087=CARTESIAN_POINT('',(-0.0025,0.00914101203113945,-0.0015));
#9088=CARTESIAN_POINT('',(0.,0.00639837134402017,0.));
#9089=CARTESIAN_POINT('',(0.,0.027,0.));
#9090=CARTESIAN_POINT('',(0.,0.0359035031847133,0.));
#9091=CARTESIAN_POINT('',(0.,0.0184403410758551,0.));
#9092=CARTESIAN_POINT('',(0.,0.0184403410758551,0.00500637669063053));
#9093=CARTESIAN_POINT('',(0.,0.0215596589241449,0.));
#9094=CARTESIAN_POINT('',(0.,0.0215596589241449,0.00500637669063053));
#9095=CARTESIAN_POINT('',(0.00803591354510047,0.0184403410758551,0.));
#9096=CARTESIAN_POINT('',(0.00803591354510047,0.0215596589241449,0.));
#9097=CARTESIAN_POINT('',(0.140895286522555,-0.0996822177859129,0.273382537537013));
#9098=CARTESIAN_POINT('',(0.,0.0075,0.));
#9099=CARTESIAN_POINT('',(0.00733163402696092,0.0075,0.00423292087906571));
#9100=CARTESIAN_POINT('',(0.00933163402696092,0.0075,0.00423292087906571));
#9101=CARTESIAN_POINT('',(0.0151423348616945,0.0075,0.00874243110855875));
#9102=CARTESIAN_POINT('',(0.0171423348616945,0.0075,0.00874243110855875));
#9103=CARTESIAN_POINT('',(0.,0.0075,0.));
#9104=CARTESIAN_POINT('',(0.0015,0.0075,-0.00259807621135332));
#9105=CARTESIAN_POINT('',(-0.0015,0.0075,0.00259807621135332));
#9106=CARTESIAN_POINT('',(-0.0015,0.0075,0.00259807621135332));
#9107=CARTESIAN_POINT('',(0.0136554445662277,0.0075,0.0113480762113533));
#9108=CARTESIAN_POINT('',(0.0151554445662277,0.0075,0.00875));
#9109=CARTESIAN_POINT('',(0.0166554445662276,0.0075,0.0061519237886467));
#9110=CARTESIAN_POINT('',(0.0015,0.0075,-0.00259807621135332));
#9111=CARTESIAN_POINT('',(0.,0.0075,0.));
#9112=CARTESIAN_POINT('',(0.,0.0075,0.0025));
#9113=CARTESIAN_POINT('',(0.,0.0065,0.));
#9114=CARTESIAN_POINT('',(0.,0.0065,0.));
#9115=CARTESIAN_POINT('',(0.0015,0.0065,-0.00259807621135332));
#9116=CARTESIAN_POINT('',(-0.0015,0.0065,0.00259807621135332));
#9117=CARTESIAN_POINT('',(0.0015,0.0065,-0.00259807621135332));
#9118=CARTESIAN_POINT('',(0.0166554445662276,0.0065,0.0061519237886467));
#9119=CARTESIAN_POINT('',(0.0151554445662277,0.0065,0.00875));
#9120=CARTESIAN_POINT('',(0.0136554445662277,0.0065,0.0113480762113533));
#9121=CARTESIAN_POINT('',(-0.0015,0.0065,0.00259807621135332));
#9122=CARTESIAN_POINT('',(0.,0.0065,0.));
#9123=CARTESIAN_POINT('',(0.,0.0065,0.0025));
#9124=CARTESIAN_POINT('',(0.,0.0075,0.));
#9125=CARTESIAN_POINT('',(-0.0015,0.0075,0.00259807621135332));
#9126=CARTESIAN_POINT('',(0.0015,0.0075,-0.00259807621135332));
#9127=CARTESIAN_POINT('',(-0.0015,0.0075,0.00259807621135332));
#9128=CARTESIAN_POINT('',(0.0136554445662277,0.0075,0.0113480762113533));
#9129=CARTESIAN_POINT('',(0.0151554445662277,0.0075,0.00875));
#9130=CARTESIAN_POINT('',(0.0166554445662276,0.0075,0.0061519237886467));
#9131=CARTESIAN_POINT('',(0.0015,0.0075,-0.00259807621135332));
#9132=CARTESIAN_POINT('',(0.,0.0075,0.));
#9133=CARTESIAN_POINT('',(0.0151423348616945,0.012,0.00874243110855875));
#9134=CARTESIAN_POINT('',(0.0151423348616945,0.012,0.00874243110855875));
#9135=CARTESIAN_POINT('',(0.0171423348616945,0.012,0.00874243110855875));
#9136=CARTESIAN_POINT('',(0.0151423348616945,0.012,0.00874243110855875));
#9137=CARTESIAN_POINT('',(0.0151423348616945,0.012,0.0102424311085587));
#9138=CARTESIAN_POINT('',(0.0151423348616945,0.012,0.00874243110855875));
#9139=CARTESIAN_POINT('',(0.0151423348616945,0.012,0.00874243110855875));
#9140=CARTESIAN_POINT('',(0.0151423348616945,0.0075,0.00874243110855875));
#9141=CARTESIAN_POINT('',(0.0151423348616945,0.0075,0.0102424311085587));
#9142=CARTESIAN_POINT('',(0.,0.0075,0.));
#9143=CARTESIAN_POINT('',(0.00733163402696092,0.012,0.00423292087906571));
#9144=CARTESIAN_POINT('',(0.00733163402696092,0.012,0.00423292087906571));
#9145=CARTESIAN_POINT('',(0.00933163402696092,0.012,0.00423292087906571));
#9146=CARTESIAN_POINT('',(0.00733163402696092,0.012,0.00423292087906571));
#9147=CARTESIAN_POINT('',(0.00733163402696092,0.012,0.0057329208790657));
#9148=CARTESIAN_POINT('',(0.00733163402696092,0.012,0.00423292087906571));
#9149=CARTESIAN_POINT('',(0.00733163402696092,0.012,0.00423292087906571));
#9150=CARTESIAN_POINT('',(0.00733163402696092,0.0075,0.00423292087906571));
#9151=CARTESIAN_POINT('',(0.00733163402696092,0.0075,0.0057329208790657));
#9152=CARTESIAN_POINT('',(0.,0.0075,0.));
#9153=CARTESIAN_POINT('',(0.132889710102238,-0.0594770446550229,0.271567574957511));
#9154=CARTESIAN_POINT('',(-0.00370266623767647,-0.0055,-0.00213773534904185));
#9155=CARTESIAN_POINT('',(-0.00370266623767647,-0.0065,-0.00213773534904185));
#9156=CARTESIAN_POINT('',(-0.0074173999821892,-0.0065,0.00429637223304478));
#9157=CARTESIAN_POINT('',(-2.42942346645285E-5,-0.0065,-0.00850886254739745));
#9158=CARTESIAN_POINT('',(-0.0074173999821892,-0.0055,0.00429637223304478));
#9159=CARTESIAN_POINT('',(-0.0074173999821892,-0.0055,0.00429637223304478));
#9160=CARTESIAN_POINT('',(-0.00370266623767647,-0.0055,-0.00213773534904185));
#9161=CARTESIAN_POINT('',(-2.42942346645285E-5,-0.0055,-0.00850886254739745));
#9162=CARTESIAN_POINT('',(-2.42942346645285E-5,-0.0055,-0.00850886254739745));
#9163=CARTESIAN_POINT('',(-0.00371473374451272,-0.0055,0.00643410758208663));
#9164=CARTESIAN_POINT('',(-0.00371473374451272,-0.0065,0.00643410758208663));
#9165=CARTESIAN_POINT('',(0.015179183486316,-0.0065,0.0173425157813521));
#9166=CARTESIAN_POINT('',(0.015179183486316,-0.0055,0.0173425157813521));
#9167=CARTESIAN_POINT('',(0.015179183486316,-0.0055,0.0173425157813521));
#9168=CARTESIAN_POINT('',(-0.00371473374451272,-0.0055,0.00643410758208663));
#9169=CARTESIAN_POINT('',(0.0188939172308287,-0.0055,0.0109084081992657));
#9170=CARTESIAN_POINT('',(0.0188939172308287,-0.0065,0.0109084081992657));
#9171=CARTESIAN_POINT('',(0.0225722892338407,-0.0065,0.00453728100091018));
#9172=CARTESIAN_POINT('',(0.0225722892338407,-0.0055,0.00453728100091018));
#9173=CARTESIAN_POINT('',(0.0225722892338407,-0.0055,0.00453728100091018));
#9174=CARTESIAN_POINT('',(0.0188939172308287,-0.0055,0.0109084081992657));
#9175=CARTESIAN_POINT('',(-0.00266693662555068,-0.0055,0.00406832833985245));
#9176=CARTESIAN_POINT('',(-0.00266693662555068,-0.0055,0.00406832833985245));
#9177=CARTESIAN_POINT('',(-0.00266693662555068,-0.0055,0.00256832833985245));
#9178=CARTESIAN_POINT('',(-0.00266693662555068,-0.0065,0.00406832833985245));
#9179=CARTESIAN_POINT('',(-0.00266693662555068,-0.0065,0.00256832833985245));
#9180=CARTESIAN_POINT('',(0.00367837200301199,-0.0055,-0.00637112719835552));
#9181=CARTESIAN_POINT('',(0.00367837200301199,-0.0065,-0.00637112719835552));
#9182=CARTESIAN_POINT('',(0.00367837200301199,-0.0055,-0.00637112719835552));
#9183=CARTESIAN_POINT('',(0.0151554445662277,-0.0055,0.00875));
#9184=CARTESIAN_POINT('',(0.0151554445662277,-0.0055,0.00875));
#9185=CARTESIAN_POINT('',(0.0151554445662277,-0.0055,0.00725));
#9186=CARTESIAN_POINT('',(0.0151554445662277,-0.0065,0.00875));
#9187=CARTESIAN_POINT('',(0.0151554445662277,-0.0065,0.00725));
#9188=CARTESIAN_POINT('',(0.0178581876187029,-0.0055,0.00470234451037119));
#9189=CARTESIAN_POINT('',(0.0178581876187029,-0.0055,0.00470234451037119));
#9190=CARTESIAN_POINT('',(0.0178581876187029,-0.0055,0.00320234451037119));
#9191=CARTESIAN_POINT('',(0.0178581876187029,-0.0065,0.00470234451037119));
#9192=CARTESIAN_POINT('',(0.0178581876187029,-0.0065,0.00320234451037119));
#9193=CARTESIAN_POINT('',(0.00218980738047307,-0.0055,-0.00434379903793625));
#9194=CARTESIAN_POINT('',(0.00218980738047307,-0.0055,-0.00434379903793625));
#9195=CARTESIAN_POINT('',(0.00218980738047307,-0.0055,-0.00584379903793625));
#9196=CARTESIAN_POINT('',(0.00218980738047307,-0.0065,-0.00434379903793625));
#9197=CARTESIAN_POINT('',(0.00218980738047307,-0.0065,-0.00584379903793625));
#9198=CARTESIAN_POINT('',(0.0130014436126792,-0.0055,0.0131144718881599));
#9199=CARTESIAN_POINT('',(0.0130014436126792,-0.0055,0.0131144718881599));
#9200=CARTESIAN_POINT('',(0.0130014436126792,-0.0055,0.0116144718881599));
#9201=CARTESIAN_POINT('',(0.0130014436126792,-0.0065,0.0131144718881599));
#9202=CARTESIAN_POINT('',(0.0130014436126792,-0.0065,0.0116144718881599));
#9203=CARTESIAN_POINT('',(0.,-0.0055,0.));
#9204=CARTESIAN_POINT('',(0.,-0.0055,0.));
#9205=CARTESIAN_POINT('',(0.,-0.0055,-0.0015));
#9206=CARTESIAN_POINT('',(0.,-0.0065,0.));
#9207=CARTESIAN_POINT('',(0.,-0.0065,0.));
#9208=CARTESIAN_POINT('',(0.,-0.0065,-0.0015));
#9209=CARTESIAN_POINT('',(0.,-0.0105,0.));
#9210=CARTESIAN_POINT('',(0.126615215151473,-0.0758135287661414,0.27109644209674));
#9211=CARTESIAN_POINT('',(0.,0.0005,0.));
#9212=CARTESIAN_POINT('',(-2.76008920646131E-17,0.0005,5.55111512312578E-17));
#9213=CARTESIAN_POINT('',(-2.77539729145066E-17,0.0005,0.00250000000000011));
#9214=CARTESIAN_POINT('',(-0.00782575698925397,0.0005,-0.00322924205021303));
#9215=CARTESIAN_POINT('',(-0.00782575698925397,0.0005,-0.00156905588883643));
#9216=CARTESIAN_POINT('',(-0.0161768612294697,0.0005,-0.00667526484586793));
#9217=CARTESIAN_POINT('',(-0.0161768612294697,0.0005,-0.00522394213364568));
#9218=CARTESIAN_POINT('',(0.,0.0005,0.));
#9219=CARTESIAN_POINT('',(0.,0.0005,0.059));
#9220=CARTESIAN_POINT('',(0.,0.,0.));
#9221=CARTESIAN_POINT('',(-2.76008920646131E-17,0.,5.55111512312578E-17));
#9222=CARTESIAN_POINT('',(-2.76008920646131E-17,0.,0.00250000000000011));
#9223=CARTESIAN_POINT('',(-0.00782575698925397,0.,-0.00322924205021303));
#9224=CARTESIAN_POINT('',(-0.00782575698925397,0.,-0.00156905588883643));
#9225=CARTESIAN_POINT('',(-0.0161768612294697,0.,-0.00667526484586793));
#9226=CARTESIAN_POINT('',(-0.0161768612294697,0.,-0.00522394213364568));
#9227=CARTESIAN_POINT('',(0.,0.,0.));
#9228=CARTESIAN_POINT('',(0.,0.,0.059));
#9229=CARTESIAN_POINT('',(0.,0.0005,0.));
#9230=CARTESIAN_POINT('',(-0.0161768612294697,-0.0095,-0.00667526484586793));
#9231=CARTESIAN_POINT('',(-0.00782575698925397,-0.0095,-0.00322924205021303));
#9232=CARTESIAN_POINT('',(-2.76008920646131E-17,-0.0245,5.55111512312578E-17));
#9233=CARTESIAN_POINT('',(0.132889710102238,-0.0594770446550228,0.283567574957512));
#9234=CARTESIAN_POINT('',(0.0500000508,0.,0.));
#9235=CARTESIAN_POINT('',(0.,0.,0.));
#9236=CARTESIAN_POINT('',(0.,0.,-0.0015));
#9237=CARTESIAN_POINT('',(0.01,0.,0.));
#9238=CARTESIAN_POINT('',(0.01,0.,-0.0015));
#9239=CARTESIAN_POINT('',(0.015,0.,0.));
#9240=CARTESIAN_POINT('',(0.005,0.,0.));
#9241=CARTESIAN_POINT('',(0.005,0.,0.0025));
#9242=CARTESIAN_POINT('',(0.01,0.,0.));
#9243=CARTESIAN_POINT('',(0.01,0.,-0.0025));
#9244=CARTESIAN_POINT('',(0.005,0.,0.));
#9245=CARTESIAN_POINT('',(0.005,0.00175014931247276,0.00486296201856249));
#9246=CARTESIAN_POINT('',(0.005,-0.000449829019689083,0.00485319789963747));
#9247=CARTESIAN_POINT('',(0.005,-0.000134141743660394,0.00599850031196196));
#9248=CARTESIAN_POINT('',(0.005,0.,0.));
#9249=CARTESIAN_POINT('',(0.005,-0.000935696069402783,0.00478334076412126));
#9250=CARTESIAN_POINT('',(0.005,-0.00304931069140626,0.00417290384710763));
#9251=CARTESIAN_POINT('',(0.005,-0.00156126476959266,0.00579331099797247));
#9252=CARTESIAN_POINT('',(0.005,0.,0.));
#9253=CARTESIAN_POINT('',(0.005,-0.0018186808906137,0.00571772680513126));
#9254=CARTESIAN_POINT('',(0.005,0.000309201244781488,0.0051590519284221));
#9255=CARTESIAN_POINT('',(0.005,-0.0017989116368419,0.00452987780440431));
#9256=CARTESIAN_POINT('',(0.005,0.,0.));
#9257=CARTESIAN_POINT('',(0.005,-0.0022454166277504,0.00432596580751883));
#9258=CARTESIAN_POINT('',(0.005,-0.00410143505307095,0.00314478182317488));
#9259=CARTESIAN_POINT('',(0.005,-0.00313018689641237,0.00511878208107439));
#9260=CARTESIAN_POINT('',(0.005,0.,0.));
#9261=CARTESIAN_POINT('',(0.005,-0.00335588132792122,0.00497373707717946));
#9262=CARTESIAN_POINT('',(0.005,-0.00115679646887138,0.00503718613310417));
#9263=CARTESIAN_POINT('',(0.005,-0.00300225713171722,0.00383957394967893));
#9264=CARTESIAN_POINT('',(0.005,0.,0.));
#9265=CARTESIAN_POINT('',(0.005,-0.00337322688492455,0.0035181268287005));
#9266=CARTESIAN_POINT('',(0.005,-0.00482128553890929,0.00186188827866615));
#9267=CARTESIAN_POINT('',(0.005,-0.00444551989682302,0.00402955988253688));
#9268=CARTESIAN_POINT('',(0.005,0.,0.));
#9269=CARTESIAN_POINT('',(0.005,-0.00462120821823529,0.00382680475118794));
#9270=CARTESIAN_POINT('',(0.005,-0.00252907741234978,0.00450723747458156));
#9271=CARTESIAN_POINT('',(0.005,-0.00396237760889148,0.00283821064837608));
#9272=CARTESIAN_POINT('',(0.005,0.,0.));
#9273=CARTESIAN_POINT('',(0.005,-0.00422775836123484,0.00242527013732674));
#9274=CARTESIAN_POINT('',(0.005,-0.00515054414367435,0.000428155618895829));
#9275=CARTESIAN_POINT('',(0.005,-0.0054007033137179,0.00261388670703158));
#9276=CARTESIAN_POINT('',(0.005,0.,0.));
#9277=CARTESIAN_POINT('',(0.005,-0.00551215230209144,0.00236984746313935));
#9278=CARTESIAN_POINT('',(0.005,-0.00369646754488213,0.00361213924144174));
#9279=CARTESIAN_POINT('',(0.005,-0.00460148981736036,0.00160691239983047));
#9280=CARTESIAN_POINT('',(0.005,0.,0.));
#9281=CARTESIAN_POINT('',(0.005,-0.004739781998565,0.00113593248306364));
#9282=CARTESIAN_POINT('',(0.005,-0.00506253629338438,-0.00104026366277791));
#9283=CARTESIAN_POINT('',(0.005,-0.0059183538673547,0.000986451975905413));
#9284=CARTESIAN_POINT('',(0.005,0.,0.));
#9285=CARTESIAN_POINT('',(0.005,-0.00595653458846414,0.000720899227652746));
#9286=CARTESIAN_POINT('',(0.005,-0.00456439186066708,0.00242440696917955));
#9287=CARTESIAN_POINT('',(0.005,-0.00486781668694036,0.000245431665326605));
#9288=CARTESIAN_POINT('',(0.005,0.,0.));
#9289=CARTESIAN_POINT('',(0.005,-0.00486781668694036,-0.000245431665326668));
#9290=CARTESIAN_POINT('',(0.005,-0.00456439186066704,-0.00242440696917961));
#9291=CARTESIAN_POINT('',(0.005,-0.00595653458846413,-0.000720899227652823));
#9292=CARTESIAN_POINT('',(0.005,0.,0.));
#9293=CARTESIAN_POINT('',(0.005,-0.00591835386735468,-0.000986451975905493));
#9294=CARTESIAN_POINT('',(0.005,-0.0050625362933844,0.00104026366277785));
#9295=CARTESIAN_POINT('',(0.005,-0.00473978199856499,-0.00113593248306371));
#9296=CARTESIAN_POINT('',(0.005,0.,0.));
#9297=CARTESIAN_POINT('',(0.005,-0.00460148981736034,-0.00160691239983053));
#9298=CARTESIAN_POINT('',(0.005,-0.00369646754488208,-0.00361213924144179));
#9299=CARTESIAN_POINT('',(0.005,-0.00551215230209141,-0.00236984746313942));
#9300=CARTESIAN_POINT('',(0.005,0.,0.));
#9301=CARTESIAN_POINT('',(0.005,-0.00540070331371787,-0.00261388670703166));
#9302=CARTESIAN_POINT('',(0.005,-0.00515054414367434,-0.0004281556188959));
#9303=CARTESIAN_POINT('',(0.005,-0.00422775836123482,-0.0024252701373268));
#9304=CARTESIAN_POINT('',(0.005,0.,0.));
#9305=CARTESIAN_POINT('',(0.005,-0.00396237760889144,-0.00283821064837614));
#9306=CARTESIAN_POINT('',(0.005,-0.00252907741234972,-0.00450723747458159));
#9307=CARTESIAN_POINT('',(0.005,-0.00462120821823524,-0.003826804751188));
#9308=CARTESIAN_POINT('',(0.005,0.,0.));
#9309=CARTESIAN_POINT('',(0.005,-0.00444551989682297,-0.00402955988253693));
#9310=CARTESIAN_POINT('',(0.005,-0.00482128553890927,-0.00186188827866621));
#9311=CARTESIAN_POINT('',(0.005,-0.0033732268849245,-0.00351812682870055));
#9312=CARTESIAN_POINT('',(0.005,0.,0.));
#9313=CARTESIAN_POINT('',(0.005,-0.00300225713171717,-0.00383957394967897));
#9314=CARTESIAN_POINT('',(0.005,-0.00115679646887131,-0.00503718613310418));
#9315=CARTESIAN_POINT('',(0.005,-0.00335588132792115,-0.00497373707717951));
#9316=CARTESIAN_POINT('',(0.005,0.,0.));
#9317=CARTESIAN_POINT('',(0.005,-0.0031301868964123,-0.00511878208107443));
#9318=CARTESIAN_POINT('',(0.005,-0.0041014350530709,-0.00314478182317494));
#9319=CARTESIAN_POINT('',(0.005,-0.00224541662775034,-0.00432596580751886));
#9320=CARTESIAN_POINT('',(0.005,0.,0.));
#9321=CARTESIAN_POINT('',(0.005,-0.00179891163684184,-0.00452987780440433));
#9322=CARTESIAN_POINT('',(0.005,0.000309201244781555,-0.0051590519284221));
#9323=CARTESIAN_POINT('',(0.005,-0.00181868089061363,-0.00571772680513128));
#9324=CARTESIAN_POINT('',(0.005,0.,0.));
#9325=CARTESIAN_POINT('',(0.005,-0.00156126476959258,-0.00579331099797249));
#9326=CARTESIAN_POINT('',(0.005,-0.0030493106914062,-0.00417290384710767));
#9327=CARTESIAN_POINT('',(0.005,-0.000935696069402719,-0.00478334076412128));
#9328=CARTESIAN_POINT('',(0.005,0.,0.));
#9329=CARTESIAN_POINT('',(0.005,-0.000449829019689018,-0.00485319789963748));
#9330=CARTESIAN_POINT('',(0.005,0.00175014931247283,-0.00486296201856246));
#9331=CARTESIAN_POINT('',(0.005,-0.000134141743660314,-0.00599850031196196));
#9332=CARTESIAN_POINT('',(0.005,0.,0.));
#9333=CARTESIAN_POINT('',(0.005,0.000134141743660434,-0.00599850031196196));
#9334=CARTESIAN_POINT('',(0.005,-0.00175014931247273,-0.0048629620185625));
#9335=CARTESIAN_POINT('',(0.005,0.000449829019689116,-0.00485319789963747));
#9336=CARTESIAN_POINT('',(0.005,0.,0.));
#9337=CARTESIAN_POINT('',(0.005,0.000935696069402815,-0.00478334076412126));
#9338=CARTESIAN_POINT('',(0.005,0.00304931069140629,-0.00417290384710761));
#9339=CARTESIAN_POINT('',(0.005,0.00156126476959269,-0.00579331099797246));
#9340=CARTESIAN_POINT('',(0.005,0.,0.));
#9341=CARTESIAN_POINT('',(0.005,0.00181868089061374,-0.00571772680513125));
#9342=CARTESIAN_POINT('',(0.005,-0.000309201244781452,-0.0051590519284221));
#9343=CARTESIAN_POINT('',(0.005,0.00179891163684193,-0.0045298778044043));
#9344=CARTESIAN_POINT('',(0.005,0.,0.));
#9345=CARTESIAN_POINT('',(0.005,0.00224541662775043,-0.00432596580751882));
#9346=CARTESIAN_POINT('',(0.005,0.00410143505307097,-0.00314478182317485));
#9347=CARTESIAN_POINT('',(0.005,0.0031301868964124,-0.00511878208107437));
#9348=CARTESIAN_POINT('',(0.005,0.,0.));
#9349=CARTESIAN_POINT('',(0.005,0.00335588132792125,-0.00497373707717944));
#9350=CARTESIAN_POINT('',(0.005,0.00115679646887141,-0.00503718613310416));
#9351=CARTESIAN_POINT('',(0.005,0.00300225713171725,-0.00383957394967891));
#9352=CARTESIAN_POINT('',(0.005,0.,0.));
#9353=CARTESIAN_POINT('',(0.005,0.00337322688492458,-0.00351812682870047));
#9354=CARTESIAN_POINT('',(0.005,0.0048212855389093,-0.00186188827866611));
#9355=CARTESIAN_POINT('',(0.005,0.00444551989682306,-0.00402955988253685));
#9356=CARTESIAN_POINT('',(0.005,0.,0.));
#9357=CARTESIAN_POINT('',(0.005,0.00462120821823532,-0.00382680475118791));
#9358=CARTESIAN_POINT('',(0.005,0.00252907741234981,-0.00450723747458154));
#9359=CARTESIAN_POINT('',(0.005,0.0039623776088915,-0.00283821064837605));
#9360=CARTESIAN_POINT('',(0.005,0.,0.));
#9361=CARTESIAN_POINT('',(0.005,0.00422775836123486,-0.00242527013732671));
#9362=CARTESIAN_POINT('',(0.005,0.00515054414367435,-0.000428155618895793));
#9363=CARTESIAN_POINT('',(0.005,0.00540070331371792,-0.00261388670703155));
#9364=CARTESIAN_POINT('',(0.005,0.,0.));
#9365=CARTESIAN_POINT('',(0.005,0.00551215230209146,-0.00236984746313931));
#9366=CARTESIAN_POINT('',(0.005,0.00369646754488215,-0.00361213924144172));
#9367=CARTESIAN_POINT('',(0.005,0.00460148981736037,-0.00160691239983044));
#9368=CARTESIAN_POINT('',(0.005,0.,0.));
#9369=CARTESIAN_POINT('',(0.005,0.00473978199856501,-0.00113593248306361));
#9370=CARTESIAN_POINT('',(0.005,0.00506253629338438,0.00104026366277795));
#9371=CARTESIAN_POINT('',(0.005,0.0059183538673547,-0.000986451975905376));
#9372=CARTESIAN_POINT('',(0.005,0.,0.));
#9373=CARTESIAN_POINT('',(0.005,0.00595653458846413,-0.000720899227652784));
#9374=CARTESIAN_POINT('',(0.005,0.00456439186066706,-0.00242440696917958));
#9375=CARTESIAN_POINT('',(0.005,0.00486781668694036,-0.000245431665326637));
#9376=CARTESIAN_POINT('',(0.005,0.,0.));
#9377=CARTESIAN_POINT('',(0.005,0.00486781668694036,0.000245431665326637));
#9378=CARTESIAN_POINT('',(0.005,0.00456439186066706,0.00242440696917958));
#9379=CARTESIAN_POINT('',(0.005,0.00595653458846413,0.000720899227652784));
#9380=CARTESIAN_POINT('',(0.005,0.,0.));
#9381=CARTESIAN_POINT('',(0.005,0.00591835386735469,0.000986451975905453));
#9382=CARTESIAN_POINT('',(0.005,0.00506253629338439,-0.00104026366277788));
#9383=CARTESIAN_POINT('',(0.005,0.004739781998565,0.00113593248306367));
#9384=CARTESIAN_POINT('',(0.005,0.,0.));
#9385=CARTESIAN_POINT('',(0.005,0.00460148981736035,0.0016069123998305));
#9386=CARTESIAN_POINT('',(0.005,0.0036964675448821,0.00361213924144177));
#9387=CARTESIAN_POINT('',(0.005,0.00551215230209143,0.00236984746313938));
#9388=CARTESIAN_POINT('',(0.005,0.,0.));
#9389=CARTESIAN_POINT('',(0.005,0.00540070331371789,0.00261388670703162));
#9390=CARTESIAN_POINT('',(0.005,0.00515054414367435,0.000428155618895864));
#9391=CARTESIAN_POINT('',(0.005,0.00422775836123483,0.00242527013732677));
#9392=CARTESIAN_POINT('',(0.005,0.,0.));
#9393=CARTESIAN_POINT('',(0.005,0.00396237760889146,0.00283821064837611));
#9394=CARTESIAN_POINT('',(0.005,0.00252907741234975,0.00450723747458157));
#9395=CARTESIAN_POINT('',(0.005,0.00462120821823527,0.00382680475118797));
#9396=CARTESIAN_POINT('',(0.005,0.,0.));
#9397=CARTESIAN_POINT('',(0.005,0.004445519896823,0.0040295598825369));
#9398=CARTESIAN_POINT('',(0.005,0.00482128553890928,0.00186188827866618));
#9399=CARTESIAN_POINT('',(0.005,0.00337322688492453,0.00351812682870053));
#9400=CARTESIAN_POINT('',(0.005,0.,0.));
#9401=CARTESIAN_POINT('',(0.005,0.0030022571317172,0.00383957394967895));
#9402=CARTESIAN_POINT('',(0.005,0.00115679646887134,0.00503718613310418));
#9403=CARTESIAN_POINT('',(0.005,0.00335588132792118,0.00497373707717948));
#9404=CARTESIAN_POINT('',(0.005,0.,0.));
#9405=CARTESIAN_POINT('',(0.005,0.00313018689641234,0.00511878208107441));
#9406=CARTESIAN_POINT('',(0.005,0.00410143505307092,0.00314478182317491));
#9407=CARTESIAN_POINT('',(0.005,0.00224541662775037,0.00432596580751884));
#9408=CARTESIAN_POINT('',(0.005,0.,0.));
#9409=CARTESIAN_POINT('',(0.005,0.00179891163684187,0.00452987780440432));
#9410=CARTESIAN_POINT('',(0.005,-0.000309201244781521,0.0051590519284221));
#9411=CARTESIAN_POINT('',(0.005,0.00181868089061367,0.00571772680513127));
#9412=CARTESIAN_POINT('',(0.005,0.,0.));
#9413=CARTESIAN_POINT('',(0.005,0.00156126476959262,0.00579331099797248));
#9414=CARTESIAN_POINT('',(0.005,0.00304931069140623,0.00417290384710765));
#9415=CARTESIAN_POINT('',(0.005,0.00093569606940275,0.00478334076412127));
#9416=CARTESIAN_POINT('',(0.005,0.,0.));
#9417=CARTESIAN_POINT('',(0.005,0.00044982901968905,0.00485319789963748));
#9418=CARTESIAN_POINT('',(0.005,-0.00175014931247279,0.00486296201856248));
#9419=CARTESIAN_POINT('',(0.005,0.000134141743660354,0.00599850031196196));
#9420=CARTESIAN_POINT('',(0.005,0.,0.));
#9421=CARTESIAN_POINT('',(-0.01,0.,0.));
#9422=CARTESIAN_POINT('',(0.0025,-0.000134141743660394,0.00599850031196196));
#9423=CARTESIAN_POINT('',(0.,-0.000134141743660394,0.00599850031196196));
#9424=CARTESIAN_POINT('',(0.0025,0.000134141743660354,0.00599850031196196));
#9425=CARTESIAN_POINT('',(0.,0.000134141743660354,0.00599850031196196));
#9426=CARTESIAN_POINT('',(0.,0.,0.));
#9427=CARTESIAN_POINT('',(-0.01,0.,0.));
#9428=CARTESIAN_POINT('',(0.0025,-0.00156126476959266,0.00579331099797247));
#9429=CARTESIAN_POINT('',(0.,-0.00156126476959266,0.00579331099797247));
#9430=CARTESIAN_POINT('',(0.,0.,0.));
#9431=CARTESIAN_POINT('',(0.,-0.0018186808906137,0.00571772680513126));
#9432=CARTESIAN_POINT('',(0.0025,-0.0018186808906137,0.00571772680513126));
#9433=CARTESIAN_POINT('',(-0.01,0.,0.));
#9434=CARTESIAN_POINT('',(0.0025,0.00156126476959262,0.00579331099797248));
#9435=CARTESIAN_POINT('',(0.,0.00156126476959262,0.00579331099797248));
#9436=CARTESIAN_POINT('',(0.0025,0.00181868089061367,0.00571772680513127));
#9437=CARTESIAN_POINT('',(0.,0.00181868089061367,0.00571772680513127));
#9438=CARTESIAN_POINT('',(0.,0.,0.));
#9439=CARTESIAN_POINT('',(-0.01,0.,0.));
#9440=CARTESIAN_POINT('',(0.0025,0.00313018689641234,0.00511878208107441));
#9441=CARTESIAN_POINT('',(0.,0.00313018689641234,0.00511878208107441));
#9442=CARTESIAN_POINT('',(0.0025,0.00335588132792118,0.00497373707717949));
#9443=CARTESIAN_POINT('',(0.,0.00335588132792118,0.00497373707717949));
#9444=CARTESIAN_POINT('',(0.,0.,0.));
#9445=CARTESIAN_POINT('',(-0.01,0.,0.));
#9446=CARTESIAN_POINT('',(0.0025,0.00540070331371789,0.00261388670703162));
#9447=CARTESIAN_POINT('',(0.,0.00540070331371789,0.00261388670703162));
#9448=CARTESIAN_POINT('',(0.0025,0.00551215230209143,0.00236984746313938));
#9449=CARTESIAN_POINT('',(0.,0.00551215230209143,0.00236984746313938));
#9450=CARTESIAN_POINT('',(0.,0.,0.));
#9451=CARTESIAN_POINT('',(-0.01,0.,0.));
#9452=CARTESIAN_POINT('',(0.0025,0.00462120821823527,0.00382680475118797));
#9453=CARTESIAN_POINT('',(0.,0.00462120821823527,0.00382680475118797));
#9454=CARTESIAN_POINT('',(0.,0.,0.));
#9455=CARTESIAN_POINT('',(0.,0.004445519896823,0.0040295598825369));
#9456=CARTESIAN_POINT('',(0.0025,0.004445519896823,0.0040295598825369));
#9457=CARTESIAN_POINT('',(-0.01,0.,0.));
#9458=CARTESIAN_POINT('',(0.0025,-0.00595653458846414,0.000720899227652746));
#9459=CARTESIAN_POINT('',(0.,-0.00595653458846414,0.000720899227652745));
#9460=CARTESIAN_POINT('',(0.0025,-0.0059183538673547,0.000986451975905412));
#9461=CARTESIAN_POINT('',(0.,-0.0059183538673547,0.000986451975905412));
#9462=CARTESIAN_POINT('',(0.,0.,0.));
#9463=CARTESIAN_POINT('',(-0.01,0.,0.));
#9464=CARTESIAN_POINT('',(0.0025,-0.00595653458846413,-0.000720899227652823));
#9465=CARTESIAN_POINT('',(0.,-0.00595653458846413,-0.000720899227652823));
#9466=CARTESIAN_POINT('',(0.,0.,0.));
#9467=CARTESIAN_POINT('',(0.,-0.00591835386735468,-0.000986451975905493));
#9468=CARTESIAN_POINT('',(0.0025,-0.00591835386735468,-0.000986451975905493));
#9469=CARTESIAN_POINT('',(-0.01,0.,0.));
#9470=CARTESIAN_POINT('',(0.0025,-0.00551215230209144,0.00236984746313935));
#9471=CARTESIAN_POINT('',(0.,-0.00551215230209144,0.00236984746313935));
#9472=CARTESIAN_POINT('',(0.0025,-0.0054007033137179,0.00261388670703158));
#9473=CARTESIAN_POINT('',(0.,-0.0054007033137179,0.00261388670703158));
#9474=CARTESIAN_POINT('',(0.,0.,0.));
#9475=CARTESIAN_POINT('',(-0.01,0.,0.));
#9476=CARTESIAN_POINT('',(0.0025,-0.00462120821823529,0.00382680475118794));
#9477=CARTESIAN_POINT('',(0.,-0.00462120821823529,0.00382680475118794));
#9478=CARTESIAN_POINT('',(0.0025,-0.00444551989682302,0.00402955988253688));
#9479=CARTESIAN_POINT('',(0.,-0.00444551989682302,0.00402955988253688));
#9480=CARTESIAN_POINT('',(0.,0.,0.));
#9481=CARTESIAN_POINT('',(-0.01,0.,0.));
#9482=CARTESIAN_POINT('',(0.0025,-0.00313018689641237,0.00511878208107439));
#9483=CARTESIAN_POINT('',(0.,-0.00313018689641237,0.00511878208107439));
#9484=CARTESIAN_POINT('',(0.,0.,0.));
#9485=CARTESIAN_POINT('',(0.,-0.00335588132792122,0.00497373707717946));
#9486=CARTESIAN_POINT('',(0.0025,-0.00335588132792122,0.00497373707717946));
#9487=CARTESIAN_POINT('',(-0.01,0.,0.));
#9488=CARTESIAN_POINT('',(0.0025,-0.00444551989682297,-0.00402955988253693));
#9489=CARTESIAN_POINT('',(0.,-0.00444551989682297,-0.00402955988253693));
#9490=CARTESIAN_POINT('',(0.0025,-0.00462120821823524,-0.00382680475118801));
#9491=CARTESIAN_POINT('',(0.,-0.00462120821823524,-0.00382680475118801));
#9492=CARTESIAN_POINT('',(0.,0.,0.));
#9493=CARTESIAN_POINT('',(-0.01,0.,0.));
#9494=CARTESIAN_POINT('',(0.0025,-0.00335588132792115,-0.00497373707717951));
#9495=CARTESIAN_POINT('',(0.,-0.00335588132792115,-0.00497373707717951));
#9496=CARTESIAN_POINT('',(0.,0.,0.));
#9497=CARTESIAN_POINT('',(0.,-0.00313018689641231,-0.00511878208107443));
#9498=CARTESIAN_POINT('',(0.0025,-0.00313018689641231,-0.00511878208107443));
#9499=CARTESIAN_POINT('',(-0.01,0.,0.));
#9500=CARTESIAN_POINT('',(0.0025,-0.00181868089061363,-0.00571772680513128));
#9501=CARTESIAN_POINT('',(0.,-0.00181868089061363,-0.00571772680513128));
#9502=CARTESIAN_POINT('',(0.,0.,0.));
#9503=CARTESIAN_POINT('',(0.,-0.00156126476959258,-0.00579331099797249));
#9504=CARTESIAN_POINT('',(0.0025,-0.00156126476959258,-0.00579331099797249));
#9505=CARTESIAN_POINT('',(-0.01,0.,0.));
#9506=CARTESIAN_POINT('',(0.0025,-0.000134141743660315,-0.00599850031196196));
#9507=CARTESIAN_POINT('',(0.,-0.000134141743660315,-0.00599850031196196));
#9508=CARTESIAN_POINT('',(0.,0.,0.));
#9509=CARTESIAN_POINT('',(0.,0.000134141743660435,-0.00599850031196196));
#9510=CARTESIAN_POINT('',(0.0025,0.000134141743660435,-0.00599850031196196));
#9511=CARTESIAN_POINT('',(-0.01,0.,0.));
#9512=CARTESIAN_POINT('',(0.0025,-0.00540070331371787,-0.00261388670703166));
#9513=CARTESIAN_POINT('',(0.,-0.00540070331371787,-0.00261388670703166));
#9514=CARTESIAN_POINT('',(0.0025,-0.00551215230209141,-0.00236984746313942));
#9515=CARTESIAN_POINT('',(0.,-0.00551215230209141,-0.00236984746313941));
#9516=CARTESIAN_POINT('',(0.,0.,0.));
#9517=CARTESIAN_POINT('',(-0.01,0.,0.));
#9518=CARTESIAN_POINT('',(0.0025,0.00335588132792125,-0.00497373707717944));
#9519=CARTESIAN_POINT('',(0.,0.00335588132792125,-0.00497373707717944));
#9520=CARTESIAN_POINT('',(0.0025,0.0031301868964124,-0.00511878208107437));
#9521=CARTESIAN_POINT('',(0.,0.0031301868964124,-0.00511878208107437));
#9522=CARTESIAN_POINT('',(0.,0.,0.));
#9523=CARTESIAN_POINT('',(-0.01,0.,0.));
#9524=CARTESIAN_POINT('',(0.0025,0.00444551989682306,-0.00402955988253685));
#9525=CARTESIAN_POINT('',(0.,0.00444551989682306,-0.00402955988253685));
#9526=CARTESIAN_POINT('',(0.,0.,0.));
#9527=CARTESIAN_POINT('',(0.,0.00462120821823532,-0.00382680475118791));
#9528=CARTESIAN_POINT('',(0.0025,0.00462120821823532,-0.00382680475118791));
#9529=CARTESIAN_POINT('',(-0.01,0.,0.));
#9530=CARTESIAN_POINT('',(0.0025,0.00540070331371792,-0.00261388670703155));
#9531=CARTESIAN_POINT('',(0.,0.00540070331371792,-0.00261388670703155));
#9532=CARTESIAN_POINT('',(0.,0.,0.));
#9533=CARTESIAN_POINT('',(0.,0.00551215230209146,-0.00236984746313931));
#9534=CARTESIAN_POINT('',(0.0025,0.00551215230209146,-0.00236984746313931));
#9535=CARTESIAN_POINT('',(-0.01,0.,0.));
#9536=CARTESIAN_POINT('',(0.0025,0.0059183538673547,-0.000986451975905377));
#9537=CARTESIAN_POINT('',(0.,0.0059183538673547,-0.000986451975905377));
#9538=CARTESIAN_POINT('',(0.,0.,0.));
#9539=CARTESIAN_POINT('',(0.,0.00595653458846413,-0.000720899227652784));
#9540=CARTESIAN_POINT('',(0.0025,0.00595653458846413,-0.000720899227652784));
#9541=CARTESIAN_POINT('',(-0.01,0.,0.));
#9542=CARTESIAN_POINT('',(0.0025,0.00181868089061374,-0.00571772680513125));
#9543=CARTESIAN_POINT('',(0.,0.00181868089061374,-0.00571772680513125));
#9544=CARTESIAN_POINT('',(0.0025,0.00156126476959269,-0.00579331099797246));
#9545=CARTESIAN_POINT('',(0.,0.00156126476959269,-0.00579331099797246));
#9546=CARTESIAN_POINT('',(0.,0.,0.));
#9547=CARTESIAN_POINT('',(0.,0.,0.));
#9548=CARTESIAN_POINT('',(0.,0.00175014931247276,0.00486296201856249));
#9549=CARTESIAN_POINT('',(0.,-0.000449829019689083,0.00485319789963747));
#9550=CARTESIAN_POINT('',(0.,-0.00175014931247279,0.00486296201856248));
#9551=CARTESIAN_POINT('',(0.,0.00044982901968905,0.00485319789963748));
#9552=CARTESIAN_POINT('',(0.,0.,0.));
#9553=CARTESIAN_POINT('',(0.,0.00093569606940275,0.00478334076412127));
#9554=CARTESIAN_POINT('',(0.,0.00304931069140623,0.00417290384710765));
#9555=CARTESIAN_POINT('',(0.,-0.000309201244781521,0.0051590519284221));
#9556=CARTESIAN_POINT('',(0.,0.00179891163684187,0.00452987780440432));
#9557=CARTESIAN_POINT('',(0.,0.,0.));
#9558=CARTESIAN_POINT('',(0.,0.00224541662775037,0.00432596580751884));
#9559=CARTESIAN_POINT('',(0.,0.00410143505307092,0.00314478182317491));
#9560=CARTESIAN_POINT('',(0.,0.00115679646887134,0.00503718613310418));
#9561=CARTESIAN_POINT('',(0.,0.0030022571317172,0.00383957394967895));
#9562=CARTESIAN_POINT('',(0.,0.,0.));
#9563=CARTESIAN_POINT('',(0.,0.00337322688492453,0.00351812682870052));
#9564=CARTESIAN_POINT('',(0.,0.00482128553890928,0.00186188827866618));
#9565=CARTESIAN_POINT('',(0.,0.00252907741234975,0.00450723747458157));
#9566=CARTESIAN_POINT('',(0.,0.00396237760889146,0.00283821064837611));
#9567=CARTESIAN_POINT('',(0.,0.,0.));
#9568=CARTESIAN_POINT('',(0.,0.00422775836123483,0.00242527013732677));
#9569=CARTESIAN_POINT('',(0.,0.00515054414367435,0.000428155618895864));
#9570=CARTESIAN_POINT('',(0.,0.0036964675448821,0.00361213924144177));
#9571=CARTESIAN_POINT('',(0.,0.00460148981736035,0.0016069123998305));
#9572=CARTESIAN_POINT('',(0.,0.,0.));
#9573=CARTESIAN_POINT('',(0.,0.004739781998565,0.00113593248306367));
#9574=CARTESIAN_POINT('',(0.,0.00506253629338439,-0.00104026366277788));
#9575=CARTESIAN_POINT('',(0.,0.00591835386735469,0.000986451975905453));
#9576=CARTESIAN_POINT('',(0.,0.,0.));
#9577=CARTESIAN_POINT('',(0.,0.00595653458846413,0.000720899227652784));
#9578=CARTESIAN_POINT('',(0.,0.00456439186066706,0.00242440696917958));
#9579=CARTESIAN_POINT('',(0.,0.00486781668694036,0.000245431665326637));
#9580=CARTESIAN_POINT('',(0.,0.,0.));
#9581=CARTESIAN_POINT('',(0.,0.00486781668694036,-0.000245431665326637));
#9582=CARTESIAN_POINT('',(0.,0.00456439186066706,-0.00242440696917958));
#9583=CARTESIAN_POINT('',(0.,0.00506253629338438,0.00104026366277795));
#9584=CARTESIAN_POINT('',(0.,0.00473978199856501,-0.00113593248306361));
#9585=CARTESIAN_POINT('',(0.,0.,0.));
#9586=CARTESIAN_POINT('',(0.,0.00460148981736037,-0.00160691239983044));
#9587=CARTESIAN_POINT('',(0.,0.00369646754488215,-0.00361213924144172));
#9588=CARTESIAN_POINT('',(0.,0.00515054414367435,-0.000428155618895793));
#9589=CARTESIAN_POINT('',(0.,0.00422775836123486,-0.00242527013732671));
#9590=CARTESIAN_POINT('',(0.,0.,0.));
#9591=CARTESIAN_POINT('',(0.,0.0039623776088915,-0.00283821064837605));
#9592=CARTESIAN_POINT('',(0.,0.00252907741234981,-0.00450723747458154));
#9593=CARTESIAN_POINT('',(0.,0.0048212855389093,-0.00186188827866611));
#9594=CARTESIAN_POINT('',(0.,0.00337322688492458,-0.00351812682870047));
#9595=CARTESIAN_POINT('',(0.,0.,0.));
#9596=CARTESIAN_POINT('',(0.,0.00300225713171725,-0.00383957394967891));
#9597=CARTESIAN_POINT('',(0.,0.00115679646887141,-0.00503718613310416));
#9598=CARTESIAN_POINT('',(0.,0.00410143505307097,-0.00314478182317485));
#9599=CARTESIAN_POINT('',(0.,0.00224541662775043,-0.00432596580751882));
#9600=CARTESIAN_POINT('',(0.,0.,0.));
#9601=CARTESIAN_POINT('',(0.,0.00179891163684193,-0.0045298778044043));
#9602=CARTESIAN_POINT('',(0.,-0.000309201244781452,-0.0051590519284221));
#9603=CARTESIAN_POINT('',(0.,0.00304931069140629,-0.00417290384710761));
#9604=CARTESIAN_POINT('',(0.,0.000935696069402815,-0.00478334076412126));
#9605=CARTESIAN_POINT('',(0.,0.,0.));
#9606=CARTESIAN_POINT('',(0.,0.000449829019689116,-0.00485319789963747));
#9607=CARTESIAN_POINT('',(0.,-0.00175014931247273,-0.0048629620185625));
#9608=CARTESIAN_POINT('',(0.,0.00175014931247283,-0.00486296201856246));
#9609=CARTESIAN_POINT('',(0.,-0.000449829019689018,-0.00485319789963748));
#9610=CARTESIAN_POINT('',(0.,0.,0.));
#9611=CARTESIAN_POINT('',(0.,-0.000935696069402719,-0.00478334076412128));
#9612=CARTESIAN_POINT('',(0.,-0.0030493106914062,-0.00417290384710767));
#9613=CARTESIAN_POINT('',(0.,0.000309201244781555,-0.0051590519284221));
#9614=CARTESIAN_POINT('',(0.,-0.00179891163684184,-0.00452987780440433));
#9615=CARTESIAN_POINT('',(0.,0.,0.));
#9616=CARTESIAN_POINT('',(0.,-0.00224541662775034,-0.00432596580751886));
#9617=CARTESIAN_POINT('',(0.,-0.0041014350530709,-0.00314478182317494));
#9618=CARTESIAN_POINT('',(0.,-0.00115679646887131,-0.00503718613310418));
#9619=CARTESIAN_POINT('',(0.,-0.00300225713171717,-0.00383957394967897));
#9620=CARTESIAN_POINT('',(0.,0.,0.));
#9621=CARTESIAN_POINT('',(0.,-0.0033732268849245,-0.00351812682870055));
#9622=CARTESIAN_POINT('',(0.,-0.00482128553890927,-0.00186188827866621));
#9623=CARTESIAN_POINT('',(0.,-0.00252907741234972,-0.00450723747458159));
#9624=CARTESIAN_POINT('',(0.,-0.00396237760889144,-0.00283821064837614));
#9625=CARTESIAN_POINT('',(0.,0.,0.));
#9626=CARTESIAN_POINT('',(0.,-0.00422775836123482,-0.0024252701373268));
#9627=CARTESIAN_POINT('',(0.,-0.00515054414367434,-0.0004281556188959));
#9628=CARTESIAN_POINT('',(0.,-0.00369646754488208,-0.00361213924144179));
#9629=CARTESIAN_POINT('',(0.,-0.00460148981736034,-0.00160691239983053));
#9630=CARTESIAN_POINT('',(0.,0.,0.));
#9631=CARTESIAN_POINT('',(0.,-0.00473978199856499,-0.00113593248306371));
#9632=CARTESIAN_POINT('',(0.,-0.0050625362933844,0.00104026366277785));
#9633=CARTESIAN_POINT('',(0.,-0.00456439186066704,-0.00242440696917961));
#9634=CARTESIAN_POINT('',(0.,-0.00486781668694036,-0.000245431665326668));
#9635=CARTESIAN_POINT('',(0.,0.,0.));
#9636=CARTESIAN_POINT('',(0.,-0.00486781668694036,0.000245431665326605));
#9637=CARTESIAN_POINT('',(0.,-0.00456439186066708,0.00242440696917955));
#9638=CARTESIAN_POINT('',(0.,-0.00506253629338438,-0.00104026366277791));
#9639=CARTESIAN_POINT('',(0.,-0.004739781998565,0.00113593248306364));
#9640=CARTESIAN_POINT('',(0.,0.,0.));
#9641=CARTESIAN_POINT('',(0.,-0.00460148981736036,0.00160691239983047));
#9642=CARTESIAN_POINT('',(0.,-0.00369646754488213,0.00361213924144174));
#9643=CARTESIAN_POINT('',(0.,-0.00515054414367435,0.000428155618895829));
#9644=CARTESIAN_POINT('',(0.,-0.00422775836123484,0.00242527013732674));
#9645=CARTESIAN_POINT('',(0.,0.,0.));
#9646=CARTESIAN_POINT('',(0.,-0.00396237760889148,0.00283821064837608));
#9647=CARTESIAN_POINT('',(0.,-0.00252907741234978,0.00450723747458156));
#9648=CARTESIAN_POINT('',(0.,-0.00482128553890929,0.00186188827866615));
#9649=CARTESIAN_POINT('',(0.,-0.00337322688492455,0.0035181268287005));
#9650=CARTESIAN_POINT('',(0.,0.,0.));
#9651=CARTESIAN_POINT('',(0.,-0.00300225713171722,0.00383957394967893));
#9652=CARTESIAN_POINT('',(0.,-0.00115679646887138,0.00503718613310417));
#9653=CARTESIAN_POINT('',(0.,-0.00410143505307095,0.00314478182317488));
#9654=CARTESIAN_POINT('',(0.,-0.0022454166277504,0.00432596580751883));
#9655=CARTESIAN_POINT('',(0.,0.,0.));
#9656=CARTESIAN_POINT('',(0.,-0.0017989116368419,0.00452987780440431));
#9657=CARTESIAN_POINT('',(0.,0.000309201244781488,0.0051590519284221));
#9658=CARTESIAN_POINT('',(0.,-0.00304931069140626,0.00417290384710763));
#9659=CARTESIAN_POINT('',(0.,-0.000935696069402783,0.00478334076412126));
#9660=CARTESIAN_POINT('',(0.,0.,0.));
#9661=CARTESIAN_POINT('',(-0.01,0.,0.));
#9662=CARTESIAN_POINT('',(0.0025,0.00591835386735469,0.000986451975905453));
#9663=CARTESIAN_POINT('',(0.0025,0.00595653458846413,0.000720899227652784));
#9664=CARTESIAN_POINT('',(0.005,0.00456439186066706,-0.00242440696917958));
#9665=CARTESIAN_POINT('',(0.005,0.00486781668694036,-0.000245431665326637));
#9666=CARTESIAN_POINT('',(0.005,0.00456439186066706,0.00242440696917958));
#9667=CARTESIAN_POINT('',(0.005,0.00486781668694036,0.000245431665326637));
#9668=CARTESIAN_POINT('',(0.005,0.,0.));
#9669=CARTESIAN_POINT('',(0.005,0.00506253629338439,-0.00104026366277788));
#9670=CARTESIAN_POINT('',(0.005,0.004739781998565,0.00113593248306367));
#9671=CARTESIAN_POINT('',(0.005,0.0036964675448821,0.00361213924144177));
#9672=CARTESIAN_POINT('',(0.005,0.00460148981736035,0.0016069123998305));
#9673=CARTESIAN_POINT('',(0.005,0.,0.));
#9674=CARTESIAN_POINT('',(0.005,-0.00175014931247273,-0.0048629620185625));
#9675=CARTESIAN_POINT('',(0.005,0.000449829019689116,-0.00485319789963747));
#9676=CARTESIAN_POINT('',(0.005,0.00304931069140629,-0.00417290384710761));
#9677=CARTESIAN_POINT('',(0.005,0.000935696069402815,-0.00478334076412126));
#9678=CARTESIAN_POINT('',(0.005,0.,0.));
#9679=CARTESIAN_POINT('',(0.005,-0.000309201244781452,-0.0051590519284221));
#9680=CARTESIAN_POINT('',(0.005,0.00179891163684193,-0.0045298778044043));
#9681=CARTESIAN_POINT('',(0.005,0.00410143505307097,-0.00314478182317485));
#9682=CARTESIAN_POINT('',(0.005,0.00224541662775043,-0.00432596580751882));
#9683=CARTESIAN_POINT('',(0.005,0.,0.));
#9684=CARTESIAN_POINT('',(0.005,0.00369646754488215,-0.00361213924144172));
#9685=CARTESIAN_POINT('',(0.005,0.00460148981736037,-0.00160691239983044));
#9686=CARTESIAN_POINT('',(0.005,0.00506253629338438,0.00104026366277795));
#9687=CARTESIAN_POINT('',(0.005,0.00473978199856501,-0.00113593248306361));
#9688=CARTESIAN_POINT('',(0.005,0.,0.));
#9689=CARTESIAN_POINT('',(0.005,0.00252907741234981,-0.00450723747458154));
#9690=CARTESIAN_POINT('',(0.005,0.0039623776088915,-0.00283821064837605));
#9691=CARTESIAN_POINT('',(0.005,0.00515054414367435,-0.000428155618895793));
#9692=CARTESIAN_POINT('',(0.005,0.00422775836123486,-0.00242527013732671));
#9693=CARTESIAN_POINT('',(0.005,0.,0.));
#9694=CARTESIAN_POINT('',(0.005,0.00115679646887141,-0.00503718613310416));
#9695=CARTESIAN_POINT('',(0.005,0.00300225713171725,-0.00383957394967891));
#9696=CARTESIAN_POINT('',(0.005,0.0048212855389093,-0.00186188827866611));
#9697=CARTESIAN_POINT('',(0.005,0.00337322688492458,-0.00351812682870047));
#9698=CARTESIAN_POINT('',(0.005,0.,0.));
#9699=CARTESIAN_POINT('',(0.005,-0.0050625362933844,0.00104026366277785));
#9700=CARTESIAN_POINT('',(0.005,-0.00473978199856499,-0.00113593248306371));
#9701=CARTESIAN_POINT('',(0.005,-0.00369646754488208,-0.00361213924144179));
#9702=CARTESIAN_POINT('',(0.005,-0.00460148981736034,-0.00160691239983053));
#9703=CARTESIAN_POINT('',(0.005,0.,0.));
#9704=CARTESIAN_POINT('',(0.005,-0.00515054414367434,-0.0004281556188959));
#9705=CARTESIAN_POINT('',(0.005,-0.00422775836123482,-0.0024252701373268));
#9706=CARTESIAN_POINT('',(0.005,-0.00252907741234972,-0.00450723747458159));
#9707=CARTESIAN_POINT('',(0.005,-0.00396237760889144,-0.00283821064837614));
#9708=CARTESIAN_POINT('',(0.005,0.,0.));
#9709=CARTESIAN_POINT('',(0.005,-0.0030493106914062,-0.00417290384710767));
#9710=CARTESIAN_POINT('',(0.005,-0.000935696069402719,-0.00478334076412128));
#9711=CARTESIAN_POINT('',(0.005,0.00175014931247283,-0.00486296201856246));
#9712=CARTESIAN_POINT('',(0.005,-0.000449829019689018,-0.00485319789963748));
#9713=CARTESIAN_POINT('',(0.005,0.,0.));
#9714=CARTESIAN_POINT('',(0.005,-0.0041014350530709,-0.00314478182317494));
#9715=CARTESIAN_POINT('',(0.005,-0.00224541662775034,-0.00432596580751886));
#9716=CARTESIAN_POINT('',(0.005,0.000309201244781555,-0.0051590519284221));
#9717=CARTESIAN_POINT('',(0.005,-0.00179891163684184,-0.00452987780440433));
#9718=CARTESIAN_POINT('',(0.005,0.,0.));
#9719=CARTESIAN_POINT('',(0.005,-0.00482128553890927,-0.00186188827866621));
#9720=CARTESIAN_POINT('',(0.005,-0.0033732268849245,-0.00351812682870055));
#9721=CARTESIAN_POINT('',(0.005,-0.00115679646887131,-0.00503718613310418));
#9722=CARTESIAN_POINT('',(0.005,-0.00300225713171717,-0.00383957394967897));
#9723=CARTESIAN_POINT('',(0.005,0.,0.));
#9724=CARTESIAN_POINT('',(0.005,-0.00115679646887138,0.00503718613310417));
#9725=CARTESIAN_POINT('',(0.005,-0.00300225713171722,0.00383957394967893));
#9726=CARTESIAN_POINT('',(0.005,-0.00482128553890929,0.00186188827866615));
#9727=CARTESIAN_POINT('',(0.005,-0.00337322688492455,0.0035181268287005));
#9728=CARTESIAN_POINT('',(0.005,0.,0.));
#9729=CARTESIAN_POINT('',(0.005,0.000309201244781488,0.0051590519284221));
#9730=CARTESIAN_POINT('',(0.005,-0.0017989116368419,0.00452987780440431));
#9731=CARTESIAN_POINT('',(0.005,-0.00410143505307095,0.00314478182317488));
#9732=CARTESIAN_POINT('',(0.005,-0.0022454166277504,0.00432596580751883));
#9733=CARTESIAN_POINT('',(0.005,0.,0.));
#9734=CARTESIAN_POINT('',(0.005,-0.00252907741234978,0.00450723747458156));
#9735=CARTESIAN_POINT('',(0.005,-0.00396237760889148,0.00283821064837608));
#9736=CARTESIAN_POINT('',(0.005,-0.00515054414367435,0.000428155618895829));
#9737=CARTESIAN_POINT('',(0.005,-0.00422775836123484,0.00242527013732674));
#9738=CARTESIAN_POINT('',(0.005,0.,0.));
#9739=CARTESIAN_POINT('',(0.005,-0.00369646754488213,0.00361213924144174));
#9740=CARTESIAN_POINT('',(0.005,-0.00460148981736036,0.00160691239983047));
#9741=CARTESIAN_POINT('',(0.005,-0.00506253629338438,-0.00104026366277791));
#9742=CARTESIAN_POINT('',(0.005,-0.004739781998565,0.00113593248306364));
#9743=CARTESIAN_POINT('',(0.005,0.,0.));
#9744=CARTESIAN_POINT('',(0.005,-0.00456439186066708,0.00242440696917955));
#9745=CARTESIAN_POINT('',(0.005,-0.00486781668694036,0.000245431665326605));
#9746=CARTESIAN_POINT('',(0.005,-0.00456439186066704,-0.00242440696917961));
#9747=CARTESIAN_POINT('',(0.005,-0.00486781668694036,-0.000245431665326668));
#9748=CARTESIAN_POINT('',(0.005,0.,0.));
#9749=CARTESIAN_POINT('',(0.005,0.00482128553890928,0.00186188827866618));
#9750=CARTESIAN_POINT('',(0.005,0.00337322688492453,0.00351812682870053));
#9751=CARTESIAN_POINT('',(0.005,0.00115679646887134,0.00503718613310418));
#9752=CARTESIAN_POINT('',(0.005,0.0030022571317172,0.00383957394967895));
#9753=CARTESIAN_POINT('',(0.005,0.,0.));
#9754=CARTESIAN_POINT('',(0.005,0.00515054414367435,0.000428155618895864));
#9755=CARTESIAN_POINT('',(0.005,0.00422775836123483,0.00242527013732677));
#9756=CARTESIAN_POINT('',(0.005,0.00252907741234975,0.00450723747458157));
#9757=CARTESIAN_POINT('',(0.005,0.00396237760889146,0.00283821064837611));
#9758=CARTESIAN_POINT('',(0.005,0.,0.));
#9759=CARTESIAN_POINT('',(0.005,0.00410143505307092,0.00314478182317491));
#9760=CARTESIAN_POINT('',(0.005,0.00224541662775037,0.00432596580751884));
#9761=CARTESIAN_POINT('',(0.005,-0.000309201244781521,0.0051590519284221));
#9762=CARTESIAN_POINT('',(0.005,0.00179891163684187,0.00452987780440432));
#9763=CARTESIAN_POINT('',(0.005,0.,0.));
#9764=CARTESIAN_POINT('',(0.005,0.00304931069140623,0.00417290384710765));
#9765=CARTESIAN_POINT('',(0.005,0.00093569606940275,0.00478334076412127));
#9766=CARTESIAN_POINT('',(0.005,-0.00175014931247279,0.00486296201856248));
#9767=CARTESIAN_POINT('',(0.005,0.00044982901968905,0.00485319789963748));
#9768=CARTESIAN_POINT('',(0.005,0.,0.));
#9769=CARTESIAN_POINT('',(0.005,0.00175014931247276,0.00486296201856249));
#9770=CARTESIAN_POINT('',(0.005,-0.000449829019689083,0.00485319789963747));
#9771=CARTESIAN_POINT('',(0.005,-0.00304931069140626,0.00417290384710763));
#9772=CARTESIAN_POINT('',(0.005,-0.000935696069402783,0.00478334076412126));
#9773=CARTESIAN_POINT('',(0.005,0.,0.));
#9774=CARTESIAN_POINT('',(0.013,0.,0.));
#9775=CARTESIAN_POINT('',(0.013,0.,0.));
#9776=CARTESIAN_POINT('',(0.013,0.,-0.0025));
#9777=CARTESIAN_POINT('',(0.013,0.,0.));
#9778=CARTESIAN_POINT('',(0.013,0.,-0.00375738138352587));
#9779=CARTESIAN_POINT('',(0.01,0.,0.));
#9780=CARTESIAN_POINT('',(0.01,0.,0.));
#9781=CARTESIAN_POINT('',(0.01,0.,-0.00375738138352587));
#9782=CARTESIAN_POINT('',(0.01,0.,0.));
#9783=CARTESIAN_POINT('',(0.01,0.,0.));
#9784=CARTESIAN_POINT('',(0.0500000508,0.,0.));
#9785=CARTESIAN_POINT('',(0.013,0.,0.));
#9786=CARTESIAN_POINT('',(0.013,0.,-0.0015));
#9787=CARTESIAN_POINT('',(0.015,0.,0.));
#9788=CARTESIAN_POINT('',(0.015,0.,-0.0015));
#9789=CARTESIAN_POINT('',(0.015,0.,0.));
#9790=CARTESIAN_POINT('',(0.015,0.,0.));
#9791=CARTESIAN_POINT('',(0.015,0.,-0.0025));
#9792=CARTESIAN_POINT('',(0.015,0.,0.));
#9793=CARTESIAN_POINT('',(0.013,0.,0.));
#9794=CARTESIAN_POINT('',(0.132889710102238,-0.0594770446550229,0.270567574957511));
#9795=CARTESIAN_POINT('',(-0.001,0.,0.));
#9796=CARTESIAN_POINT('',(0.001,0.,0.));
#9797=CARTESIAN_POINT('',(0.001,0.00174902830165781,-0.05097));
#9798=CARTESIAN_POINT('',(0.001,0.005,-0.0507543101617981));
#9799=CARTESIAN_POINT('',(-0.001,0.00174902830165781,-0.05097));
#9800=CARTESIAN_POINT('',(-0.001,0.00174902830165781,-0.05097));
#9801=CARTESIAN_POINT('',(-0.001,0.,0.));
#9802=CARTESIAN_POINT('',(-0.001,0.005,-0.0507543101617981));
#9803=CARTESIAN_POINT('',(-0.001,0.005,-0.0507543101617981));
#9804=CARTESIAN_POINT('',(-0.001,0.,-0.05));
#9805=CARTESIAN_POINT('',(0.001,0.,-0.05));
#9806=CARTESIAN_POINT('',(0.001,0.00171438035453047,-0.04897));
#9807=CARTESIAN_POINT('',(-0.001,0.00171438035453047,-0.04897));
#9808=CARTESIAN_POINT('',(-0.001,0.00171438035453047,-0.04897));
#9809=CARTESIAN_POINT('',(-0.001,0.,-0.05));
#9810=CARTESIAN_POINT('',(-0.001,0.,0.));
#9811=CARTESIAN_POINT('',(0.001,0.,0.));
#9812=CARTESIAN_POINT('',(0.001,0.005,-0.0487442304278158));
#9813=CARTESIAN_POINT('',(-0.001,0.005,-0.0487442304278158));
#9814=CARTESIAN_POINT('',(-0.001,0.005,-0.0487442304278158));
#9815=CARTESIAN_POINT('',(-0.001,0.,0.));
#9816=CARTESIAN_POINT('',(-0.001,0.005,-0.0487442304278158));
#9817=CARTESIAN_POINT('',(0.001,0.005,-0.0487442304278158));
#9818=CARTESIAN_POINT('',(-0.001,0.005,-0.0487442304278158));
#9819=CARTESIAN_POINT('',(-0.001,0.,0.));
#9820=CARTESIAN_POINT('',(-0.001,0.,-0.05));
#9821=CARTESIAN_POINT('',(-0.001,0.,-0.0515));
#9822=CARTESIAN_POINT('',(0.001,0.,0.));
#9823=CARTESIAN_POINT('',(0.001,0.,-0.05));
#9824=CARTESIAN_POINT('',(0.001,0.,-0.0515));
#9825=CARTESIAN_POINT('',(-0.001,0.,-0.05));
#9826=CARTESIAN_POINT('',(0.133528696378885,-0.0631790818800808,0.269067574957511));
#9827=CARTESIAN_POINT('',(-0.0025,0.,0.));
#9828=CARTESIAN_POINT('',(-0.0025,-0.05,6.38104651849169E-19));
#9829=CARTESIAN_POINT('',(-0.0025,-0.0485,-8.6757429628926E-20));
#9830=CARTESIAN_POINT('',(-0.0025,-0.0515,-4.84711505179759E-20));
#9831=CARTESIAN_POINT('',(-0.0025,0.,0.));
#9832=CARTESIAN_POINT('',(-0.0025,0.005,-0.0482415795761291));
#9833=CARTESIAN_POINT('',(-0.0025,0.005,-0.0512567068782223));
#9834=CARTESIAN_POINT('',(-0.00289537313791363,0.005,-0.0512567068782223));
#9835=CARTESIAN_POINT('',(-0.00367744748009773,0.005,-0.0509278560554984));
#9836=CARTESIAN_POINT('',(-0.0041616283571214,0.005,-0.0497471530643231));
#9837=CARTESIAN_POINT('',(-0.00367603360051941,0.005,-0.0485697710976327));
#9838=CARTESIAN_POINT('',(-0.00289360144208482,0.005,-0.0482415795761291));
#9839=CARTESIAN_POINT('',(-0.0025,0.005,-0.0482415795761291));
#9840=CARTESIAN_POINT('',(-0.0025,0.005,-0.0512567068782223));
#9841=CARTESIAN_POINT('',(-0.0025,0.,0.));
#9842=CARTESIAN_POINT('',(-0.0951557364069925,0.,0.));
#9843=CARTESIAN_POINT('',(-0.0951557364069925,-0.0485,-8.6757429628926E-20));
#9844=CARTESIAN_POINT('',(0.0025,-0.0485,6.18961512293694E-19));
#9845=CARTESIAN_POINT('',(0.0025,0.,0.));
#9846=CARTESIAN_POINT('',(0.0025,0.005,-0.0482415795761291));
#9847=CARTESIAN_POINT('',(-0.0951557364069925,0.005,-0.0482415795761291));
#9848=CARTESIAN_POINT('',(0.0025,0.,0.));
#9849=CARTESIAN_POINT('',(0.0025,-0.05,6.38104651849169E-19));
#9850=CARTESIAN_POINT('',(0.0025,-0.0515,-4.84711505179759E-20));
#9851=CARTESIAN_POINT('',(0.0025,0.,0.));
#9852=CARTESIAN_POINT('',(0.0025,0.005,-0.0512567068782223));
#9853=CARTESIAN_POINT('',(0.0025,0.005,-0.0482415795761291));
#9854=CARTESIAN_POINT('',(0.00289405455214165,0.005,-0.0482415795761291));
#9855=CARTESIAN_POINT('',(0.00367769277965407,0.005,-0.0485708711433478));
#9856=CARTESIAN_POINT('',(0.00416046967205458,0.005,-0.0497486705893407));
#9857=CARTESIAN_POINT('',(0.00368042750626719,0.005,-0.0509263588341051));
#9858=CARTESIAN_POINT('',(0.00289165153003374,0.005,-0.0512567068782223));
#9859=CARTESIAN_POINT('',(0.0025,0.005,-0.0512567068782223));
#9860=CARTESIAN_POINT('',(-0.0951557364069925,0.,0.));
#9861=CARTESIAN_POINT('',(-0.0951557364069925,-0.0515,-4.84711505179759E-20));
#9862=CARTESIAN_POINT('',(-0.0951557364069925,0.005,-0.0512567068782223));
#9863=CARTESIAN_POINT('',(-0.005,0.005,-7.69529407107537E-19));
#9864=CARTESIAN_POINT('',(-0.0025,0.005,-0.0522613624009172));
#9865=CARTESIAN_POINT('',(-0.00315874911763011,0.005,-0.0522613624009172));
#9866=CARTESIAN_POINT('',(-0.00446402043389959,0.005,-0.051711570220507));
#9867=CARTESIAN_POINT('',(-0.00526880926820208,0.005,-0.0497473158066496));
#9868=CARTESIAN_POINT('',(-0.00446073660632804,0.005,-0.0477820413045601));
#9869=CARTESIAN_POINT('',(-0.00315306096378925,0.005,-0.047236109069228));
#9870=CARTESIAN_POINT('',(-0.0025,0.005,-0.047236109069228));
#9871=CARTESIAN_POINT('',(-0.0025,0.005,-0.0522613624009172));
#9872=CARTESIAN_POINT('',(-0.0025,0.005,-0.047236109069228));
#9873=CARTESIAN_POINT('',(-0.0951557364069925,0.005,-0.0522613624009172));
#9874=CARTESIAN_POINT('',(0.0025,0.005,-0.0522613624009172));
#9875=CARTESIAN_POINT('',(0.0025,0.005,-0.047236109069228));
#9876=CARTESIAN_POINT('',(0.00316127281190909,0.005,-0.047236109069228));
#9877=CARTESIAN_POINT('',(0.00445940049784844,0.005,-0.0477845184982856));
#9878=CARTESIAN_POINT('',(0.0052689178838484,0.005,-0.049746449755392));
#9879=CARTESIAN_POINT('',(0.00446492217011694,0.005,-0.0517126600905919));
#9880=CARTESIAN_POINT('',(0.00315462463920908,0.005,-0.0522613624009172));
#9881=CARTESIAN_POINT('',(0.0025,0.005,-0.0522613624009172));
#9882=CARTESIAN_POINT('',(0.0025,0.005,-0.047236109069228));
#9883=CARTESIAN_POINT('',(-0.0951557364069925,0.005,-0.047236109069228));
#9884=CARTESIAN_POINT('',(-0.005,0.005,-7.69529407107537E-19));
#9885=CARTESIAN_POINT('',(-0.0025,-0.05,6.38104651849169E-19));
#9886=CARTESIAN_POINT('',(-0.0025,-0.0475,-9.95195226659094E-20));
#9887=CARTESIAN_POINT('',(-0.0025,-0.0525,-3.57090574809925E-20));
#9888=CARTESIAN_POINT('',(-0.0951557364069925,-0.0475,-9.95195226659094E-20));
#9889=CARTESIAN_POINT('',(0.0025,-0.0475,6.0619941925671E-19));
#9890=CARTESIAN_POINT('',(0.0025,-0.05,6.38104651849169E-19));
#9891=CARTESIAN_POINT('',(0.0025,-0.0525,-3.57090574809925E-20));
#9892=CARTESIAN_POINT('',(-0.0951557364069925,-0.0525,-3.57090574809925E-20));
#9893=CARTESIAN_POINT('',(-0.0025,0.,0.));
#9894=CARTESIAN_POINT('',(-0.0025,0.,0.));
#9895=CARTESIAN_POINT('',(-0.0025,0.,0.));
#9896=CARTESIAN_POINT('',(-0.0951557364069925,0.,0.));
#9897=CARTESIAN_POINT('',(0.0025,0.,0.));
#9898=CARTESIAN_POINT('',(0.0025,0.,0.));
#9899=CARTESIAN_POINT('',(0.0025,0.,0.));
#9900=CARTESIAN_POINT('',(-0.0951557364069925,0.,0.));
#9901=CARTESIAN_POINT('',(0.132889710102238,-0.0594770446550228,0.270641032570794));
#9902=CARTESIAN_POINT('',(0.,0.,0.));
#9903=CARTESIAN_POINT('',(-0.012585,0.001,0.));
#9904=CARTESIAN_POINT('',(-0.012585,0.001,0.));
#9905=CARTESIAN_POINT('',(-0.012585,0.001,0.0015));
#9906=CARTESIAN_POINT('',(-0.012585,0.001,0.));
#9907=CARTESIAN_POINT('',(-0.012585,0.001,-0.002));
#9908=CARTESIAN_POINT('',(-0.012585,0.001,0.002));
#9909=CARTESIAN_POINT('',(-0.012585,0.001,0.002));
#9910=CARTESIAN_POINT('',(0.012585,0.001,0.002));
#9911=CARTESIAN_POINT('',(0.012585,0.001,0.));
#9912=CARTESIAN_POINT('',(0.012585,0.001,-0.002));
#9913=CARTESIAN_POINT('',(-0.012585,0.001,-0.002));
#9914=CARTESIAN_POINT('',(0.012585,0.001,0.));
#9915=CARTESIAN_POINT('',(0.012585,0.001,0.0015));
#9916=CARTESIAN_POINT('',(-0.012585,0.,0.));
#9917=CARTESIAN_POINT('',(-0.012585,0.,0.));
#9918=CARTESIAN_POINT('',(-0.012585,0.,-0.002));
#9919=CARTESIAN_POINT('',(-0.012585,0.,0.002));
#9920=CARTESIAN_POINT('',(-0.012585,0.,-0.002));
#9921=CARTESIAN_POINT('',(0.012585,0.,-0.002));
#9922=CARTESIAN_POINT('',(0.012585,0.,0.));
#9923=CARTESIAN_POINT('',(0.012585,0.,0.002));
#9924=CARTESIAN_POINT('',(-0.012585,0.,0.002));
#9925=CARTESIAN_POINT('',(-0.012585,0.,0.));
#9926=CARTESIAN_POINT('',(-0.012585,0.,0.0015));
#9927=CARTESIAN_POINT('',(0.012585,0.,0.));
#9928=CARTESIAN_POINT('',(0.012585,0.,0.0015));
#9929=CARTESIAN_POINT('',(-0.012585,0.001,0.));
#9930=CARTESIAN_POINT('',(-0.012585,0.001,0.002));
#9931=CARTESIAN_POINT('',(-0.012585,0.001,-0.002));
#9932=CARTESIAN_POINT('',(-0.012585,0.001,0.002));
#9933=CARTESIAN_POINT('',(0.012585,0.001,0.002));
#9934=CARTESIAN_POINT('',(0.012585,0.001,0.));
#9935=CARTESIAN_POINT('',(0.012585,0.001,-0.002));
#9936=CARTESIAN_POINT('',(-0.012585,0.001,-0.002));
#9937=CARTESIAN_POINT('',(-0.012585,0.001,0.));
#9938=CARTESIAN_POINT('',(0.012585,0.001,0.));
#9939=CARTESIAN_POINT('',(0.09201502566934,-0.0835198129330078,0.270067574957509));
#9940=CARTESIAN_POINT('',(0.,0.0660090909090909,0.));
#9941=CARTESIAN_POINT('',(0.,0.0396535295792868,0.));
#9942=CARTESIAN_POINT('',(0.,0.0396535295792868,0.0635));
#9943=CARTESIAN_POINT('',(0.,0.0421535295792868,0.));
#9944=CARTESIAN_POINT('',(0.,0.0421535295792868,0.0635));
#9945=CARTESIAN_POINT('',(0.06,0.0421535295792868,0.));
#9946=CARTESIAN_POINT('',(0.,0.0421535295792868,0.));
#9947=CARTESIAN_POINT('',(0.,0.0421535295792868,0.06));
#9948=CARTESIAN_POINT('',(0.,0.0660090909090909,0.));
#9949=CARTESIAN_POINT('',(0.,0.0426535295792868,0.));
#9950=CARTESIAN_POINT('',(0.,0.0426535295792868,0.06));
#9951=CARTESIAN_POINT('',(0.,0.0434387048123469,0.));
#9952=CARTESIAN_POINT('',(0.,0.0434387048123469,0.));
#9953=CARTESIAN_POINT('',(0.,0.0434387048123469,0.0619081467766146));
#9954=CARTESIAN_POINT('',(0.,0.0431535295792868,0.));
#9955=CARTESIAN_POINT('',(0.,0.043251523679028,0.));
#9956=CARTESIAN_POINT('',(0.,0.043251523679028,0.0636093675261996));
#9957=CARTESIAN_POINT('',(0.,0.0660090909090909,0.));
#9958=CARTESIAN_POINT('',(0.,0.0396535295792868,0.));
#9959=CARTESIAN_POINT('',(0.,0.0396535295792868,0.0645));
#9960=CARTESIAN_POINT('',(0.,0.0422575222986401,0.));
#9961=CARTESIAN_POINT('',(0.,0.0422575222986401,-0.0645));
#9962=CARTESIAN_POINT('',(0.0619081467766146,0.0364304487369043,0.));
#9963=CARTESIAN_POINT('',(0.,0.0364304487369043,0.));
#9964=CARTESIAN_POINT('',(0.,0.0364304487369043,0.0629081467766146));
#9965=CARTESIAN_POINT('',(0.,0.0364304487369043,0.));
#9966=CARTESIAN_POINT('',(0.,0.0364304487369043,0.0644389218390369));
#9967=CARTESIAN_POINT('',(0.,0.0660090909090909,0.));
#9968=CARTESIAN_POINT('',(0.,0.0374304487369043,0.));
#9969=CARTESIAN_POINT('',(0.,0.0374304487369043,0.0619081467766146));
#9970=CARTESIAN_POINT('',(0.,0.0396535295792868,0.));
#9971=CARTESIAN_POINT('',(0.,0.0396535295792868,0.0619081467766146));
#9972=CARTESIAN_POINT('',(0.0635,0.0396535295792868,0.));
#9973=CARTESIAN_POINT('',(0.,0.0396535295792868,0.));
#9974=CARTESIAN_POINT('',(0.,0.0386745739867052,0.));
#9975=CARTESIAN_POINT('',(0.,0.0386745739867052,0.0637040733883139));
#9976=CARTESIAN_POINT('',(0.,0.0422575222986401,0.));
#9977=CARTESIAN_POINT('',(0.,0.0376956183941869,0.));
#9978=CARTESIAN_POINT('',(0.,0.0376956183941869,0.));
#9979=CARTESIAN_POINT('',(0.,0.0376956183941869,0.0629081467766146));
#9980=CARTESIAN_POINT('',(0.,0.0384304487369043,0.));
#9981=CARTESIAN_POINT('',(0.,0.0374313822435482,0.));
#9982=CARTESIAN_POINT('',(0.,0.0374313822435482,0.0635431988692856));
#9983=CARTESIAN_POINT('',(0.,0.0364323157506478,0.));
#9984=CARTESIAN_POINT('',(0.,0.0364323157506478,0.));
#9985=CARTESIAN_POINT('',(0.,0.0364323157506478,-0.0645));
#9986=CARTESIAN_POINT('',(0.,0.0374304487369043,0.));
#9987=CARTESIAN_POINT('',(0.,0.0374304487369043,0.));
#9988=CARTESIAN_POINT('',(0.132889710102238,-0.0594770446550228,0.251308716820145));
#9989=CARTESIAN_POINT('',(0.00569655549855441,0.0005,-0.000257682665739804));
#9990=CARTESIAN_POINT('',(0.00569655549855441,0.0005,-0.000257682665739804));
#9991=CARTESIAN_POINT('',(0.00569655549855441,0.0005,0.));
#9992=CARTESIAN_POINT('',(0.00581839809795156,0.0005,-0.000484739348519487));
#9993=CARTESIAN_POINT('',(0.00938954980005402,0.0005,-0.00713966843895529));
#9994=CARTESIAN_POINT('',(0.00184152090594629,0.0005,-0.00687800932508196));
#9995=CARTESIAN_POINT('',(0.00182205353244363,0.0005,-0.00743958081217945));
#9996=CARTESIAN_POINT('',(0.00182205353244363,0.0005,-0.00743958081217945));
#9997=CARTESIAN_POINT('',(0.,0.0005,-0.00915134041122065));
#9998=CARTESIAN_POINT('',(0.00169914269912228,0.0005,-0.0109851653996041));
#9999=CARTESIAN_POINT('',(0.,0.0005,-0.06));
#10000=CARTESIAN_POINT('',(0.,0.0005,-0.06));
#10001=CARTESIAN_POINT('',(0.,0.0005,-0.06));
#10002=CARTESIAN_POINT('',(-0.00169914269912228,0.0005,-0.0109851653996041));
#10003=CARTESIAN_POINT('',(0.,0.0005,-0.00915134041122065));
#10004=CARTESIAN_POINT('',(-0.00182205353244363,0.0005,-0.00743958081217945));
#10005=CARTESIAN_POINT('',(-0.00182205353244363,0.0005,-0.00743958081217945));
#10006=CARTESIAN_POINT('',(-0.0018415209059463,0.0005,-0.00687800932508196));
#10007=CARTESIAN_POINT('',(-0.00938954980005402,0.0005,-0.00713966843895529));
#10008=CARTESIAN_POINT('',(-0.00581839809795156,0.0005,-0.000484739348519492));
#10009=CARTESIAN_POINT('',(-0.00569655549855441,0.0005,-0.000257682665739804));
#10010=CARTESIAN_POINT('',(-0.00569655549855441,0.0005,0.));
#10011=CARTESIAN_POINT('',(-0.00569655549855441,0.0005,0.));
#10012=CARTESIAN_POINT('',(0.,0.0005,-0.00915134041122065));
#10013=CARTESIAN_POINT('',(0.,0.0005,-0.00765134041122065));
#10014=CARTESIAN_POINT('',(0.00569655549855441,0.,-0.000257682665739804));
#10015=CARTESIAN_POINT('',(0.00569655549855441,0.,-0.000257682665739804));
#10016=CARTESIAN_POINT('',(0.00569655549855441,0.,0.));
#10017=CARTESIAN_POINT('',(0.00581839809795156,0.,-0.000484739348519487));
#10018=CARTESIAN_POINT('',(-0.00569655549855441,0.,0.));
#10019=CARTESIAN_POINT('',(-0.00569655549855441,0.,0.));
#10020=CARTESIAN_POINT('',(-0.00569655549855441,0.,-0.000257682665739804));
#10021=CARTESIAN_POINT('',(-0.00581839809795156,0.,-0.000484739348519492));
#10022=CARTESIAN_POINT('',(-0.00938954980005402,0.,-0.00713966843895529));
#10023=CARTESIAN_POINT('',(-0.0018415209059463,0.,-0.00687800932508196));
#10024=CARTESIAN_POINT('',(-0.00182205353244363,0.,-0.00743958081217945));
#10025=CARTESIAN_POINT('',(-0.00182205353244363,0.,-0.00743958081217945));
#10026=CARTESIAN_POINT('',(0.,0.,-0.00915134041122065));
#10027=CARTESIAN_POINT('',(-0.00169914269912228,0.,-0.0109851653996041));
#10028=CARTESIAN_POINT('',(0.,0.,-0.06));
#10029=CARTESIAN_POINT('',(0.,0.,-0.06));
#10030=CARTESIAN_POINT('',(0.,0.,-0.06));
#10031=CARTESIAN_POINT('',(0.00169914269912228,0.,-0.0109851653996041));
#10032=CARTESIAN_POINT('',(0.,0.,-0.00915134041122065));
#10033=CARTESIAN_POINT('',(0.00182205353244363,0.,-0.00743958081217945));
#10034=CARTESIAN_POINT('',(0.00182205353244363,0.,-0.00743958081217945));
#10035=CARTESIAN_POINT('',(0.00184152090594629,0.,-0.00687800932508196));
#10036=CARTESIAN_POINT('',(0.00938954980005402,0.,-0.00713966843895529));
#10037=CARTESIAN_POINT('',(0.,0.,-0.00915134041122065));
#10038=CARTESIAN_POINT('',(0.,0.,-0.00765134041122065));
#10039=CARTESIAN_POINT('',(0.00569655549855441,0.0005,-0.000257682665739804));
#10040=CARTESIAN_POINT('',(0.00581839809795156,0.0005,-0.000484739348519487));
#10041=CARTESIAN_POINT('',(0.00569655549855441,0.0005,0.));
#10042=CARTESIAN_POINT('',(0.00938954980005402,0.0005,-0.00713966843895529));
#10043=CARTESIAN_POINT('',(0.00184152090594629,0.0005,-0.00687800932508196));
#10044=CARTESIAN_POINT('',(0.00182205353244363,0.0005,-0.00743958081217945));
#10045=CARTESIAN_POINT('',(0.00182205353244363,0.0005,-0.00743958081217945));
#10046=CARTESIAN_POINT('',(0.,0.0005,-0.00915134041122065));
#10047=CARTESIAN_POINT('',(0.00169914269912228,0.0005,-0.0109851653996041));
#10048=CARTESIAN_POINT('',(0.,0.0005,-0.06));
#10049=CARTESIAN_POINT('',(0.,0.0005,-0.06));
#10050=CARTESIAN_POINT('',(0.,0.0005,-0.06));
#10051=CARTESIAN_POINT('',(-0.00169914269912228,0.0005,-0.0109851653996041));
#10052=CARTESIAN_POINT('',(0.,0.0005,-0.00915134041122065));
#10053=CARTESIAN_POINT('',(-0.00182205353244363,0.0005,-0.00743958081217945));
#10054=CARTESIAN_POINT('',(-0.00182205353244363,0.0005,-0.00743958081217945));
#10055=CARTESIAN_POINT('',(-0.0018415209059463,0.0005,-0.00687800932508196));
#10056=CARTESIAN_POINT('',(-0.00938954980005402,0.0005,-0.00713966843895529));
#10057=CARTESIAN_POINT('',(-0.00581839809795156,0.0005,-0.000484739348519492));
#10058=CARTESIAN_POINT('',(-0.00569655549855441,0.0005,-0.000257682665739804));
#10059=CARTESIAN_POINT('',(-0.00569655549855441,0.0005,0.));
#10060=CARTESIAN_POINT('',(-0.00569655549855441,0.0005,0.));
#10061=CARTESIAN_POINT('',(0.,0.0005,-0.00915134041122065));
#10062=CARTESIAN_POINT('',(0.131752677443887,-0.0685574735025985,0.285567574957512));
#10063=CARTESIAN_POINT('',(-0.00104626020282667,0.,6.50521303491303E-19));
#10064=CARTESIAN_POINT('',(0.,-0.0003,6.50521303491303E-19));
#10065=CARTESIAN_POINT('',(-0.00197826943066075,-0.0003,6.50521303491303E-19));
#10066=CARTESIAN_POINT('',(0.00197826943066075,-0.0003,6.50521303491303E-19));
#10067=CARTESIAN_POINT('',(0.,0.,6.50521303491303E-19));
#10068=CARTESIAN_POINT('',(0.,0.,-0.0001));
#10069=CARTESIAN_POINT('',(0.,0.,-9.12844257252368E-5));
#10070=CARTESIAN_POINT('',(-0.00207897297737586,0.0003,-9.12844257252367E-5));
#10071=CARTESIAN_POINT('',(0.00207897297737584,0.0003,-9.12844257252368E-5));
#10072=CARTESIAN_POINT('',(-0.00207897297737584,0.0003,-9.12844257252392E-5));
#10073=CARTESIAN_POINT('',(-0.00207459712624839,0.0003,-4.17809699915527E-5));
#10074=CARTESIAN_POINT('',(-0.00202837661239549,0.0003,-6.48859435981983E-19));
#10075=CARTESIAN_POINT('',(-0.00197826943066076,0.0003,3.05634754505891E-21));
#10076=CARTESIAN_POINT('',(-0.00197826943066075,0.0003,6.50521303491303E-19));
#10077=CARTESIAN_POINT('',(0.,0.,6.50521303491303E-19));
#10078=CARTESIAN_POINT('',(0.00197826943066075,0.0003,6.50521303491303E-19));
#10079=CARTESIAN_POINT('',(0.00197826943066076,0.0003,1.75840007344507E-18));
#10080=CARTESIAN_POINT('',(0.00202795255984864,0.0003,1.11200139422846E-18));
#10081=CARTESIAN_POINT('',(0.00207460838288334,0.0003,-4.19083148928644E-5));
#10082=CARTESIAN_POINT('',(0.00207897297737584,0.0003,-9.12844257252363E-5));
#10083=CARTESIAN_POINT('',(0.,0.,-0.0039));
#10084=CARTESIAN_POINT('',(0.,0.,-0.00755643035625));
#10085=CARTESIAN_POINT('',(0.00125,0.,-0.00755643035625));
#10086=CARTESIAN_POINT('',(0.,0.,-0.0019));
#10087=CARTESIAN_POINT('',(-0.00125,0.,-0.0019));
#10088=CARTESIAN_POINT('',(-0.000625,0.,-0.0078));
#10089=CARTESIAN_POINT('',(0.,0.,-0.0078));
#10090=CARTESIAN_POINT('',(0.00100643035625,0.,-0.0078));
#10091=CARTESIAN_POINT('',(-0.00104626020282667,0.,6.50521303491303E-19));
#10092=CARTESIAN_POINT('',(-5.01008275896316E-5,0.0003,6.50521303491303E-19));
#10093=CARTESIAN_POINT('',(0.,0.,1.3010426069826E-18));
#10094=CARTESIAN_POINT('',(0.,0.,-9.12844257252368E-5));
#10095=CARTESIAN_POINT('',(0.00207897297737919,-0.0003,-9.12844257253807E-5));
#10096=CARTESIAN_POINT('',(-0.00207897297737586,-0.0003,-9.12844257252367E-5));
#10097=CARTESIAN_POINT('',(-0.00207897297737588,-0.0003,-9.12844257252349E-5));
#10098=CARTESIAN_POINT('',(-0.00209690871796292,-0.0003,-0.000294189212551694));
#10099=CARTESIAN_POINT('',(-0.00211483976375729,-0.0003,-0.000497094414503252));
#10100=CARTESIAN_POINT('',(-0.00213276646112605,-0.0003,-0.000699999999999994));
#10101=CARTESIAN_POINT('',(-0.00213276646112597,-0.0003,-0.0007));
#10102=CARTESIAN_POINT('',(0.,0.,-0.0007));
#10103=CARTESIAN_POINT('',(-0.00213276646112597,0.0003,-0.0007));
#10104=CARTESIAN_POINT('',(-0.00207897297737588,0.0003,-9.12844257252349E-5));
#10105=CARTESIAN_POINT('',(-0.00209690871796292,0.0003,-0.000294189212551693));
#10106=CARTESIAN_POINT('',(-0.00211483976375729,0.0003,-0.000497094414503251));
#10107=CARTESIAN_POINT('',(-0.00213276646112605,0.0003,-0.000699999999999993));
#10108=CARTESIAN_POINT('',(0.00213276646112605,0.0003,-0.000699999999999993));
#10109=CARTESIAN_POINT('',(0.00211483976374572,0.0003,-0.000497094414372398));
#10110=CARTESIAN_POINT('',(0.00209690871792154,0.0003,-0.000294189212083583));
#10111=CARTESIAN_POINT('',(0.00207897297737588,0.0003,-9.12844257252331E-5));
#10112=CARTESIAN_POINT('',(0.00213276646112597,0.0003,-0.0007));
#10113=CARTESIAN_POINT('',(0.,0.,-0.0007));
#10114=CARTESIAN_POINT('',(0.00213276646112597,-0.0003,-0.0007));
#10115=CARTESIAN_POINT('',(0.00213276646112605,-0.0003,-0.000699999999999993));
#10116=CARTESIAN_POINT('',(0.00211483976374574,-0.0003,-0.000497094414372544));
#10117=CARTESIAN_POINT('',(0.00209690871792157,-0.0003,-0.000294189212083876));
#10118=CARTESIAN_POINT('',(0.00207897297737592,-0.0003,-9.12844257256711E-5));
#10119=CARTESIAN_POINT('',(0.,0.,-0.0018));
#10120=CARTESIAN_POINT('',(-0.00225,0.,-0.0018));
#10121=CARTESIAN_POINT('',(-0.0018,0.,-0.0018));
#10122=CARTESIAN_POINT('',(0.,0.,-0.0018));
#10123=CARTESIAN_POINT('',(-0.00135,0.,-0.0018));
#10124=CARTESIAN_POINT('',(0.,0.,-0.0019));
#10125=CARTESIAN_POINT('',(0.,0.,-0.0001));
#10126=CARTESIAN_POINT('',(-0.00207897297737584,-0.0003,-9.12844257252392E-5));
#10127=CARTESIAN_POINT('',(-0.00207459712624839,-0.0003,-4.17809699915526E-5));
#10128=CARTESIAN_POINT('',(-0.00202837661239549,-0.0003,-6.54219152761022E-19));
#10129=CARTESIAN_POINT('',(-0.00197826943066076,-0.0003,-2.30336923397844E-21));
#10130=CARTESIAN_POINT('',(0.00197826943066075,-0.0003,1.76771743586486E-18));
#10131=CARTESIAN_POINT('',(0.00202795255984883,-0.0003,1.12131875664574E-18));
#10132=CARTESIAN_POINT('',(0.00207460838288366,-0.0003,-4.19083148932107E-5));
#10133=CARTESIAN_POINT('',(0.00207897297737589,-0.0003,-9.12844257258122E-5));
#10134=CARTESIAN_POINT('',(0.,0.,-0.0007));
#10135=CARTESIAN_POINT('',(0.,-0.0003,-0.0007));
#10136=CARTESIAN_POINT('',(-5.01008275896316E-5,0.0003,-0.0007));
#10137=CARTESIAN_POINT('',(0.,-0.0003,-0.0007));
#10138=CARTESIAN_POINT('',(-5.01008275896316E-5,0.0003,-0.0007));
#10139=CARTESIAN_POINT('',(0.,0.,-0.0078));
#10140=CARTESIAN_POINT('',(0.132889710102238,-0.0594770446550229,0.285367574957512));
#10141=MECHANICAL_DESIGN_GEOMETRIC_PRESENTATION_REPRESENTATION('',(#5553,
#5554,#5555,#5556,#5557,#5558,#5559,#5560,#5561,#5562,#5563,#5564,#5565,
#5566),#10142);
#10142=(
GEOMETRIC_REPRESENTATION_CONTEXT(3)
GLOBAL_UNCERTAINTY_ASSIGNED_CONTEXT((#10158))
GLOBAL_UNIT_ASSIGNED_CONTEXT((#10176,#10175,#10174))
REPRESENTATION_CONTEXT('MAS-674','TOP_LEVEL_ASSEMBLY_PART')
);
#10143=(
GEOMETRIC_REPRESENTATION_CONTEXT(3)
GLOBAL_UNCERTAINTY_ASSIGNED_CONTEXT((#10159))
GLOBAL_UNIT_ASSIGNED_CONTEXT((#10176,#10175,#10174))
REPRESENTATION_CONTEXT('Part 1','COMPONENT_PART')
);
#10144=(
GEOMETRIC_REPRESENTATION_CONTEXT(3)
GLOBAL_UNCERTAINTY_ASSIGNED_CONTEXT((#10160))
GLOBAL_UNIT_ASSIGNED_CONTEXT((#10176,#10175,#10174))
REPRESENTATION_CONTEXT('Slotted cheese head screw M2.5x0.45 x 10',
'COMPONENT_PART')
);
#10145=(
GEOMETRIC_REPRESENTATION_CONTEXT(3)
GLOBAL_UNCERTAINTY_ASSIGNED_CONTEXT((#10161))
GLOBAL_UNIT_ASSIGNED_CONTEXT((#10176,#10175,#10174))
REPRESENTATION_CONTEXT('Part 1','COMPONENT_PART')
);
#10146=(
GEOMETRIC_REPRESENTATION_CONTEXT(3)
GLOBAL_UNCERTAINTY_ASSIGNED_CONTEXT((#10162))
GLOBAL_UNIT_ASSIGNED_CONTEXT((#10176,#10175,#10174))
REPRESENTATION_CONTEXT('Part 1','COMPONENT_PART')
);
#10147=(
GEOMETRIC_REPRESENTATION_CONTEXT(3)
GLOBAL_UNCERTAINTY_ASSIGNED_CONTEXT((#10163))
GLOBAL_UNIT_ASSIGNED_CONTEXT((#10176,#10175,#10174))
REPRESENTATION_CONTEXT('Part 3','COMPONENT_PART')
);
#10148=(
GEOMETRIC_REPRESENTATION_CONTEXT(3)
GLOBAL_UNCERTAINTY_ASSIGNED_CONTEXT((#10164))
GLOBAL_UNIT_ASSIGNED_CONTEXT((#10176,#10175,#10174))
REPRESENTATION_CONTEXT('Part 2','COMPONENT_PART')
);
#10149=(
GEOMETRIC_REPRESENTATION_CONTEXT(3)
GLOBAL_UNCERTAINTY_ASSIGNED_CONTEXT((#10165))
GLOBAL_UNIT_ASSIGNED_CONTEXT((#10176,#10175,#10174))
REPRESENTATION_CONTEXT('Part 1','COMPONENT_PART')
);
#10150=(
GEOMETRIC_REPRESENTATION_CONTEXT(3)
GLOBAL_UNCERTAINTY_ASSIGNED_CONTEXT((#10166))
GLOBAL_UNIT_ASSIGNED_CONTEXT((#10176,#10175,#10174))
REPRESENTATION_CONTEXT('Part 1','COMPONENT_PART')
);
#10151=(
GEOMETRIC_REPRESENTATION_CONTEXT(3)
GLOBAL_UNCERTAINTY_ASSIGNED_CONTEXT((#10167))
GLOBAL_UNIT_ASSIGNED_CONTEXT((#10176,#10175,#10174))
REPRESENTATION_CONTEXT('Assembly 2 <1>','COMPONENT_PART')
);
#10152=(
GEOMETRIC_REPRESENTATION_CONTEXT(3)
GLOBAL_UNCERTAINTY_ASSIGNED_CONTEXT((#10168))
GLOBAL_UNIT_ASSIGNED_CONTEXT((#10176,#10175,#10174))
REPRESENTATION_CONTEXT('Part 2','COMPONENT_PART')
);
#10153=(
GEOMETRIC_REPRESENTATION_CONTEXT(3)
GLOBAL_UNCERTAINTY_ASSIGNED_CONTEXT((#10169))
GLOBAL_UNIT_ASSIGNED_CONTEXT((#10176,#10175,#10174))
REPRESENTATION_CONTEXT('Part 3','COMPONENT_PART')
);
#10154=(
GEOMETRIC_REPRESENTATION_CONTEXT(3)
GLOBAL_UNCERTAINTY_ASSIGNED_CONTEXT((#10170))
GLOBAL_UNIT_ASSIGNED_CONTEXT((#10176,#10175,#10174))
REPRESENTATION_CONTEXT('Part 1','COMPONENT_PART')
);
#10155=(
GEOMETRIC_REPRESENTATION_CONTEXT(3)
GLOBAL_UNCERTAINTY_ASSIGNED_CONTEXT((#10171))
GLOBAL_UNIT_ASSIGNED_CONTEXT((#10176,#10175,#10174))
REPRESENTATION_CONTEXT('Part 1','COMPONENT_PART')
);
#10156=(
GEOMETRIC_REPRESENTATION_CONTEXT(3)
GLOBAL_UNCERTAINTY_ASSIGNED_CONTEXT((#10172))
GLOBAL_UNIT_ASSIGNED_CONTEXT((#10176,#10175,#10174))
REPRESENTATION_CONTEXT('Part 1','COMPONENT_PART')
);
#10157=(
GEOMETRIC_REPRESENTATION_CONTEXT(3)
GLOBAL_UNCERTAINTY_ASSIGNED_CONTEXT((#10173))
GLOBAL_UNIT_ASSIGNED_CONTEXT((#10176,#10175,#10174))
REPRESENTATION_CONTEXT('Slotted cheese head screw M2.5x0.45 x 6',
'COMPONENT_PART')
);
#10158=UNCERTAINTY_MEASURE_WITH_UNIT(LENGTH_MEASURE(1.E-8),#10176,
'DISTANCE_ACCURACY_VALUE','Maximum Tolerance applied to model');
#10159=UNCERTAINTY_MEASURE_WITH_UNIT(LENGTH_MEASURE(2.E-5),#10176,
'DISTANCE_ACCURACY_VALUE','Maximum Tolerance applied to model');
#10160=UNCERTAINTY_MEASURE_WITH_UNIT(LENGTH_MEASURE(2.E-5),#10176,
'DISTANCE_ACCURACY_VALUE','Maximum Tolerance applied to model');
#10161=UNCERTAINTY_MEASURE_WITH_UNIT(LENGTH_MEASURE(1.E-8),#10176,
'DISTANCE_ACCURACY_VALUE','Maximum Tolerance applied to model');
#10162=UNCERTAINTY_MEASURE_WITH_UNIT(LENGTH_MEASURE(2.E-5),#10176,
'DISTANCE_ACCURACY_VALUE','Maximum Tolerance applied to model');
#10163=UNCERTAINTY_MEASURE_WITH_UNIT(LENGTH_MEASURE(1.E-8),#10176,
'DISTANCE_ACCURACY_VALUE','Maximum Tolerance applied to model');
#10164=UNCERTAINTY_MEASURE_WITH_UNIT(LENGTH_MEASURE(1.E-8),#10176,
'DISTANCE_ACCURACY_VALUE','Maximum Tolerance applied to model');
#10165=UNCERTAINTY_MEASURE_WITH_UNIT(LENGTH_MEASURE(1.E-8),#10176,
'DISTANCE_ACCURACY_VALUE','Maximum Tolerance applied to model');
#10166=UNCERTAINTY_MEASURE_WITH_UNIT(LENGTH_MEASURE(1.E-8),#10176,
'DISTANCE_ACCURACY_VALUE','Maximum Tolerance applied to model');
#10167=UNCERTAINTY_MEASURE_WITH_UNIT(LENGTH_MEASURE(1.E-8),#10176,
'DISTANCE_ACCURACY_VALUE','Maximum Tolerance applied to model');
#10168=UNCERTAINTY_MEASURE_WITH_UNIT(LENGTH_MEASURE(1.E-8),#10176,
'DISTANCE_ACCURACY_VALUE','Maximum Tolerance applied to model');
#10169=UNCERTAINTY_MEASURE_WITH_UNIT(LENGTH_MEASURE(2.E-5),#10176,
'DISTANCE_ACCURACY_VALUE','Maximum Tolerance applied to model');
#10170=UNCERTAINTY_MEASURE_WITH_UNIT(LENGTH_MEASURE(1.E-8),#10176,
'DISTANCE_ACCURACY_VALUE','Maximum Tolerance applied to model');
#10171=UNCERTAINTY_MEASURE_WITH_UNIT(LENGTH_MEASURE(1.E-8),#10176,
'DISTANCE_ACCURACY_VALUE','Maximum Tolerance applied to model');
#10172=UNCERTAINTY_MEASURE_WITH_UNIT(LENGTH_MEASURE(1.E-8),#10176,
'DISTANCE_ACCURACY_VALUE','Maximum Tolerance applied to model');
#10173=UNCERTAINTY_MEASURE_WITH_UNIT(LENGTH_MEASURE(2.E-5),#10176,
'DISTANCE_ACCURACY_VALUE','Maximum Tolerance applied to model');
#10174=(
NAMED_UNIT(*)
SI_UNIT($,.STERADIAN.)
SOLID_ANGLE_UNIT()
);
#10175=(
NAMED_UNIT(*)
PLANE_ANGLE_UNIT()
SI_UNIT($,.RADIAN.)
);
#10176=(
LENGTH_UNIT()
NAMED_UNIT(*)
SI_UNIT($,.METRE.)
);
#10177=PRODUCT_DEFINITION_SHAPE('','',#10210);
#10178=PRODUCT_DEFINITION_SHAPE('','',#10211);
#10179=PRODUCT_DEFINITION_SHAPE(' ','NAUO PRDDFN',#620);
#10180=PRODUCT_DEFINITION_SHAPE('','',#10212);
#10181=PRODUCT_DEFINITION_SHAPE(' ','NAUO PRDDFN',#621);
#10182=PRODUCT_DEFINITION_SHAPE(' ','NAUO PRDDFN',#622);
#10183=PRODUCT_DEFINITION_SHAPE('','',#10213);
#10184=PRODUCT_DEFINITION_SHAPE(' ','NAUO PRDDFN',#623);
#10185=PRODUCT_DEFINITION_SHAPE(' ','NAUO PRDDFN',#624);
#10186=PRODUCT_DEFINITION_SHAPE('','',#10214);
#10187=PRODUCT_DEFINITION_SHAPE(' ','NAUO PRDDFN',#625);
#10188=PRODUCT_DEFINITION_SHAPE('','',#10215);
#10189=PRODUCT_DEFINITION_SHAPE(' ','NAUO PRDDFN',#626);
#10190=PRODUCT_DEFINITION_SHAPE('','',#10216);
#10191=PRODUCT_DEFINITION_SHAPE(' ','NAUO PRDDFN',#627);
#10192=PRODUCT_DEFINITION_SHAPE('','',#10217);
#10193=PRODUCT_DEFINITION_SHAPE(' ','NAUO PRDDFN',#628);
#10194=PRODUCT_DEFINITION_SHAPE('','',#10218);
#10195=PRODUCT_DEFINITION_SHAPE(' ','NAUO PRDDFN',#629);
#10196=PRODUCT_DEFINITION_SHAPE('','',#10219);
#10197=PRODUCT_DEFINITION_SHAPE('','',#10220);
#10198=PRODUCT_DEFINITION_SHAPE(' ','NAUO PRDDFN',#630);
#10199=PRODUCT_DEFINITION_SHAPE('','',#10221);
#10200=PRODUCT_DEFINITION_SHAPE(' ','NAUO PRDDFN',#631);
#10201=PRODUCT_DEFINITION_SHAPE(' ','NAUO PRDDFN',#632);
#10202=PRODUCT_DEFINITION_SHAPE('','',#10222);
#10203=PRODUCT_DEFINITION_SHAPE(' ','NAUO PRDDFN',#633);
#10204=PRODUCT_DEFINITION_SHAPE('','',#10223);
#10205=PRODUCT_DEFINITION_SHAPE(' ','NAUO PRDDFN',#634);
#10206=PRODUCT_DEFINITION_SHAPE('','',#10224);
#10207=PRODUCT_DEFINITION_SHAPE(' ','NAUO PRDDFN',#635);
#10208=PRODUCT_DEFINITION_SHAPE('','',#10225);
#10209=PRODUCT_DEFINITION_SHAPE(' ','NAUO PRDDFN',#636);
#10210=PRODUCT_DEFINITION('','',#10242,#10226);
#10211=PRODUCT_DEFINITION('','',#10243,#10227);
#10212=PRODUCT_DEFINITION('','',#10244,#10228);
#10213=PRODUCT_DEFINITION('','',#10245,#10229);
#10214=PRODUCT_DEFINITION('','',#10246,#10230);
#10215=PRODUCT_DEFINITION('','',#10247,#10231);
#10216=PRODUCT_DEFINITION('','',#10248,#10232);
#10217=PRODUCT_DEFINITION('','',#10249,#10233);
#10218=PRODUCT_DEFINITION('','',#10250,#10234);
#10219=PRODUCT_DEFINITION('','',#10251,#10235);
#10220=PRODUCT_DEFINITION('','',#10252,#10236);
#10221=PRODUCT_DEFINITION('','',#10253,#10237);
#10222=PRODUCT_DEFINITION('','',#10254,#10238);
#10223=PRODUCT_DEFINITION('','',#10255,#10239);
#10224=PRODUCT_DEFINITION('','',#10256,#10240);
#10225=PRODUCT_DEFINITION('','',#10257,#10241);
#10226=PRODUCT_DEFINITION_CONTEXT('',#10323,'design');
#10227=PRODUCT_DEFINITION_CONTEXT('',#10323,'design');
#10228=PRODUCT_DEFINITION_CONTEXT('',#10323,'design');
#10229=PRODUCT_DEFINITION_CONTEXT('',#10323,'design');
#10230=PRODUCT_DEFINITION_CONTEXT('',#10323,'design');
#10231=PRODUCT_DEFINITION_CONTEXT('',#10323,'design');
#10232=PRODUCT_DEFINITION_CONTEXT('',#10323,'design');
#10233=PRODUCT_DEFINITION_CONTEXT('',#10323,'design');
#10234=PRODUCT_DEFINITION_CONTEXT('',#10323,'design');
#10235=PRODUCT_DEFINITION_CONTEXT('',#10323,'design');
#10236=PRODUCT_DEFINITION_CONTEXT('',#10323,'design');
#10237=PRODUCT_DEFINITION_CONTEXT('',#10323,'design');
#10238=PRODUCT_DEFINITION_CONTEXT('',#10323,'design');
#10239=PRODUCT_DEFINITION_CONTEXT('',#10323,'design');
#10240=PRODUCT_DEFINITION_CONTEXT('',#10323,'design');
#10241=PRODUCT_DEFINITION_CONTEXT('',#10323,'design');
#10242=PRODUCT_DEFINITION_FORMATION_WITH_SPECIFIED_SOURCE('','',#10274,
 .NOT_KNOWN.);
#10243=PRODUCT_DEFINITION_FORMATION_WITH_SPECIFIED_SOURCE('','',#10275,
 .NOT_KNOWN.);
#10244=PRODUCT_DEFINITION_FORMATION_WITH_SPECIFIED_SOURCE('','',#10276,
 .NOT_KNOWN.);
#10245=PRODUCT_DEFINITION_FORMATION_WITH_SPECIFIED_SOURCE('','',#10277,
 .NOT_KNOWN.);
#10246=PRODUCT_DEFINITION_FORMATION_WITH_SPECIFIED_SOURCE('','',#10278,
 .NOT_KNOWN.);
#10247=PRODUCT_DEFINITION_FORMATION_WITH_SPECIFIED_SOURCE('','',#10279,
 .NOT_KNOWN.);
#10248=PRODUCT_DEFINITION_FORMATION_WITH_SPECIFIED_SOURCE('','',#10280,
 .NOT_KNOWN.);
#10249=PRODUCT_DEFINITION_FORMATION_WITH_SPECIFIED_SOURCE('','',#10281,
 .NOT_KNOWN.);
#10250=PRODUCT_DEFINITION_FORMATION_WITH_SPECIFIED_SOURCE('','',#10282,
 .NOT_KNOWN.);
#10251=PRODUCT_DEFINITION_FORMATION_WITH_SPECIFIED_SOURCE('','',#10283,
 .NOT_KNOWN.);
#10252=PRODUCT_DEFINITION_FORMATION_WITH_SPECIFIED_SOURCE('','',#10284,
 .NOT_KNOWN.);
#10253=PRODUCT_DEFINITION_FORMATION_WITH_SPECIFIED_SOURCE('','',#10285,
 .NOT_KNOWN.);
#10254=PRODUCT_DEFINITION_FORMATION_WITH_SPECIFIED_SOURCE('','',#10286,
 .NOT_KNOWN.);
#10255=PRODUCT_DEFINITION_FORMATION_WITH_SPECIFIED_SOURCE('','',#10287,
 .NOT_KNOWN.);
#10256=PRODUCT_DEFINITION_FORMATION_WITH_SPECIFIED_SOURCE('','',#10288,
 .NOT_KNOWN.);
#10257=PRODUCT_DEFINITION_FORMATION_WITH_SPECIFIED_SOURCE('','',#10289,
 .NOT_KNOWN.);
#10258=PRODUCT_RELATED_PRODUCT_CATEGORY('','',(#10274));
#10259=PRODUCT_RELATED_PRODUCT_CATEGORY('','',(#10275));
#10260=PRODUCT_RELATED_PRODUCT_CATEGORY('','',(#10276));
#10261=PRODUCT_RELATED_PRODUCT_CATEGORY('','',(#10277));
#10262=PRODUCT_RELATED_PRODUCT_CATEGORY('','',(#10278));
#10263=PRODUCT_RELATED_PRODUCT_CATEGORY('','',(#10279));
#10264=PRODUCT_RELATED_PRODUCT_CATEGORY('','',(#10280));
#10265=PRODUCT_RELATED_PRODUCT_CATEGORY('','',(#10281));
#10266=PRODUCT_RELATED_PRODUCT_CATEGORY('','',(#10282));
#10267=PRODUCT_RELATED_PRODUCT_CATEGORY('','',(#10283));
#10268=PRODUCT_RELATED_PRODUCT_CATEGORY('','',(#10284));
#10269=PRODUCT_RELATED_PRODUCT_CATEGORY('','',(#10285));
#10270=PRODUCT_RELATED_PRODUCT_CATEGORY('','',(#10286));
#10271=PRODUCT_RELATED_PRODUCT_CATEGORY('','',(#10287));
#10272=PRODUCT_RELATED_PRODUCT_CATEGORY('','',(#10288));
#10273=PRODUCT_RELATED_PRODUCT_CATEGORY('','',(#10289));
#10274=PRODUCT('MAS-674','MAS-674','MAS-674',(#10306));
#10275=PRODUCT('Part 1','Part 1','Part 1',(#10307));
#10276=PRODUCT('Slotted cheese head screw M2.5x0.45 x 10',
'Slotted cheese head screw M2.5x0.45 x 10',
'Slotted cheese head screw M2.5x0.45 x 10',(#10308));
#10277=PRODUCT('Part 1','Part 1','Part 1',(#10309));
#10278=PRODUCT('Part 1','Part 1','Part 1',(#10310));
#10279=PRODUCT('Part 3','Part 3','Part 3',(#10311));
#10280=PRODUCT('Part 2','Part 2','Part 2',(#10312));
#10281=PRODUCT('Part 1','Part 1','Part 1',(#10313));
#10282=PRODUCT('Part 1','Part 1','Part 1',(#10314));
#10283=PRODUCT('Assembly 2 <1>','Assembly 2 <1>','Assembly 2 <1>',(#10315));
#10284=PRODUCT('Part 2','Part 2','Part 2',(#10316));
#10285=PRODUCT('Part 3','Part 3','Part 3',(#10317));
#10286=PRODUCT('Part 1','Part 1','Part 1',(#10318));
#10287=PRODUCT('Part 1','Part 1','Part 1',(#10319));
#10288=PRODUCT('Part 1','Part 1','Part 1',(#10320));
#10289=PRODUCT('Slotted cheese head screw M2.5x0.45 x 6',
'Slotted cheese head screw M2.5x0.45 x 6',
'Slotted cheese head screw M2.5x0.45 x 6',(#10321));
#10290=PRODUCT_CATEGORY('','');
#10291=PRODUCT_CATEGORY('','');
#10292=PRODUCT_CATEGORY('','');
#10293=PRODUCT_CATEGORY('','');
#10294=PRODUCT_CATEGORY('','');
#10295=PRODUCT_CATEGORY('','');
#10296=PRODUCT_CATEGORY('','');
#10297=PRODUCT_CATEGORY('','');
#10298=PRODUCT_CATEGORY('','');
#10299=PRODUCT_CATEGORY('','');
#10300=PRODUCT_CATEGORY('','');
#10301=PRODUCT_CATEGORY('','');
#10302=PRODUCT_CATEGORY('','');
#10303=PRODUCT_CATEGORY('','');
#10304=PRODUCT_CATEGORY('','');
#10305=PRODUCT_CATEGORY('','');
#10306=PRODUCT_CONTEXT('',#10323,'mechanical');
#10307=PRODUCT_CONTEXT('',#10323,'mechanical');
#10308=PRODUCT_CONTEXT('',#10323,'mechanical');
#10309=PRODUCT_CONTEXT('',#10323,'mechanical');
#10310=PRODUCT_CONTEXT('',#10323,'mechanical');
#10311=PRODUCT_CONTEXT('',#10323,'mechanical');
#10312=PRODUCT_CONTEXT('',#10323,'mechanical');
#10313=PRODUCT_CONTEXT('',#10323,'mechanical');
#10314=PRODUCT_CONTEXT('',#10323,'mechanical');
#10315=PRODUCT_CONTEXT('',#10323,'mechanical');
#10316=PRODUCT_CONTEXT('',#10323,'mechanical');
#10317=PRODUCT_CONTEXT('',#10323,'mechanical');
#10318=PRODUCT_CONTEXT('',#10323,'mechanical');
#10319=PRODUCT_CONTEXT('',#10323,'mechanical');
#10320=PRODUCT_CONTEXT('',#10323,'mechanical');
#10321=PRODUCT_CONTEXT('',#10323,'mechanical');
#10322=APPLICATION_PROTOCOL_DEFINITION('international standard',
'ap242_managed_model_based_3d_engineering',2020,#10323);
#10323=APPLICATION_CONTEXT('managed model based 3d engineering');
ENDSEC;
END-ISO-10303-21;
